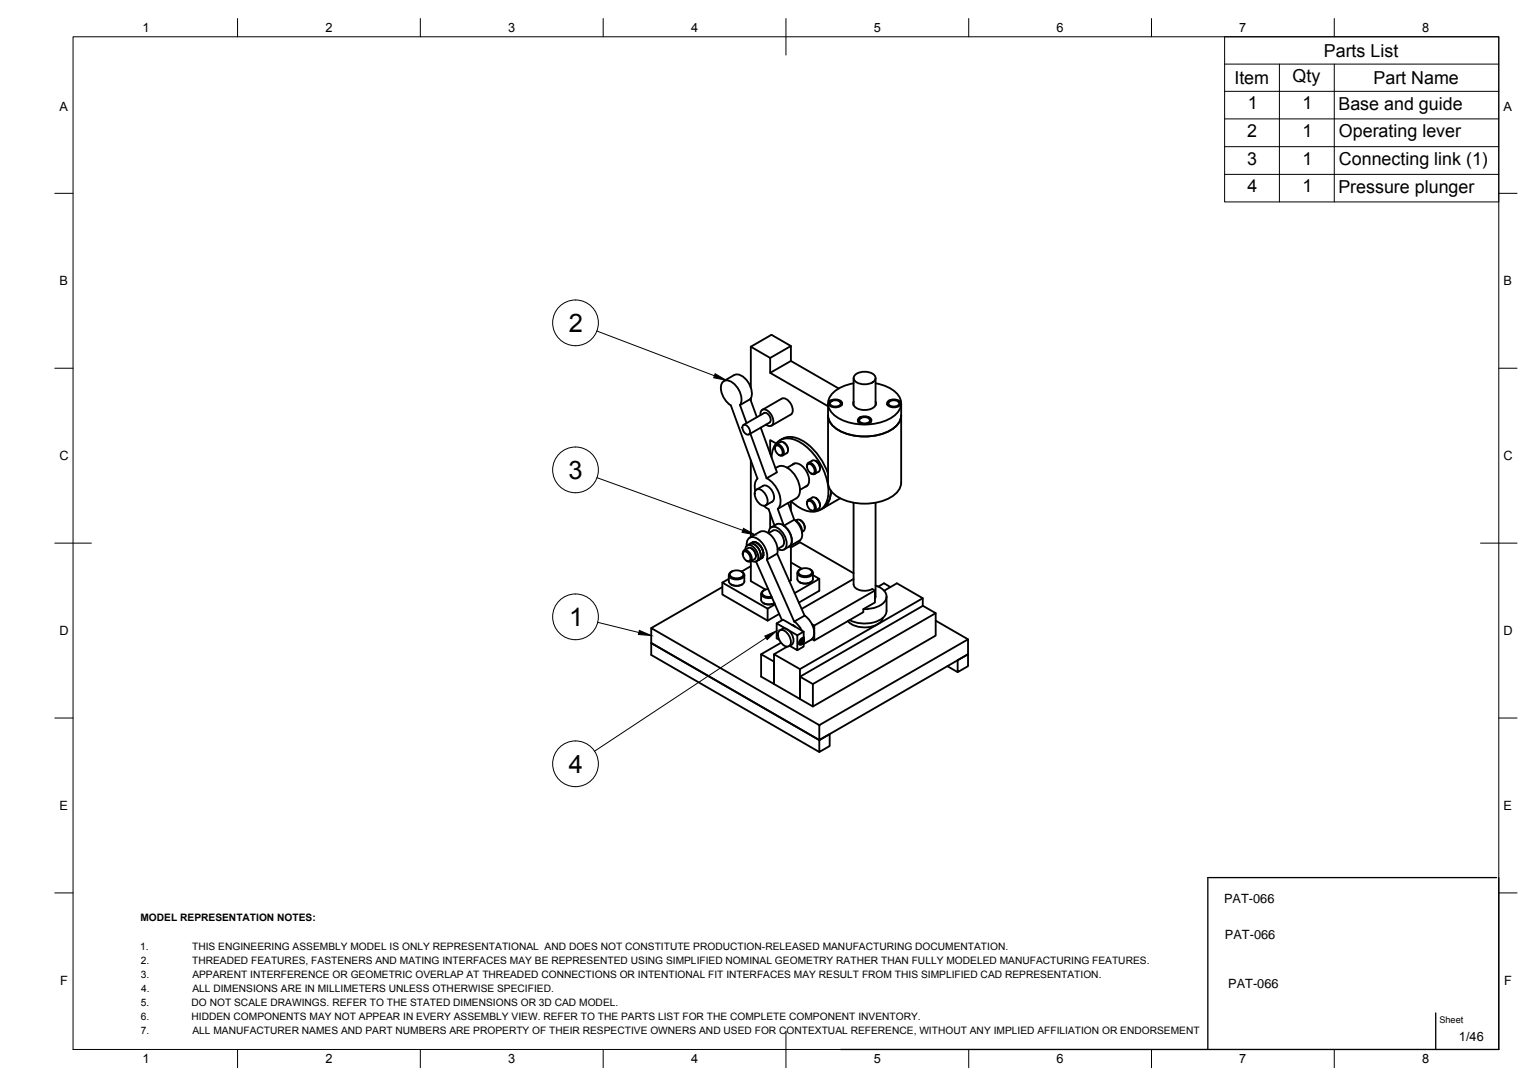
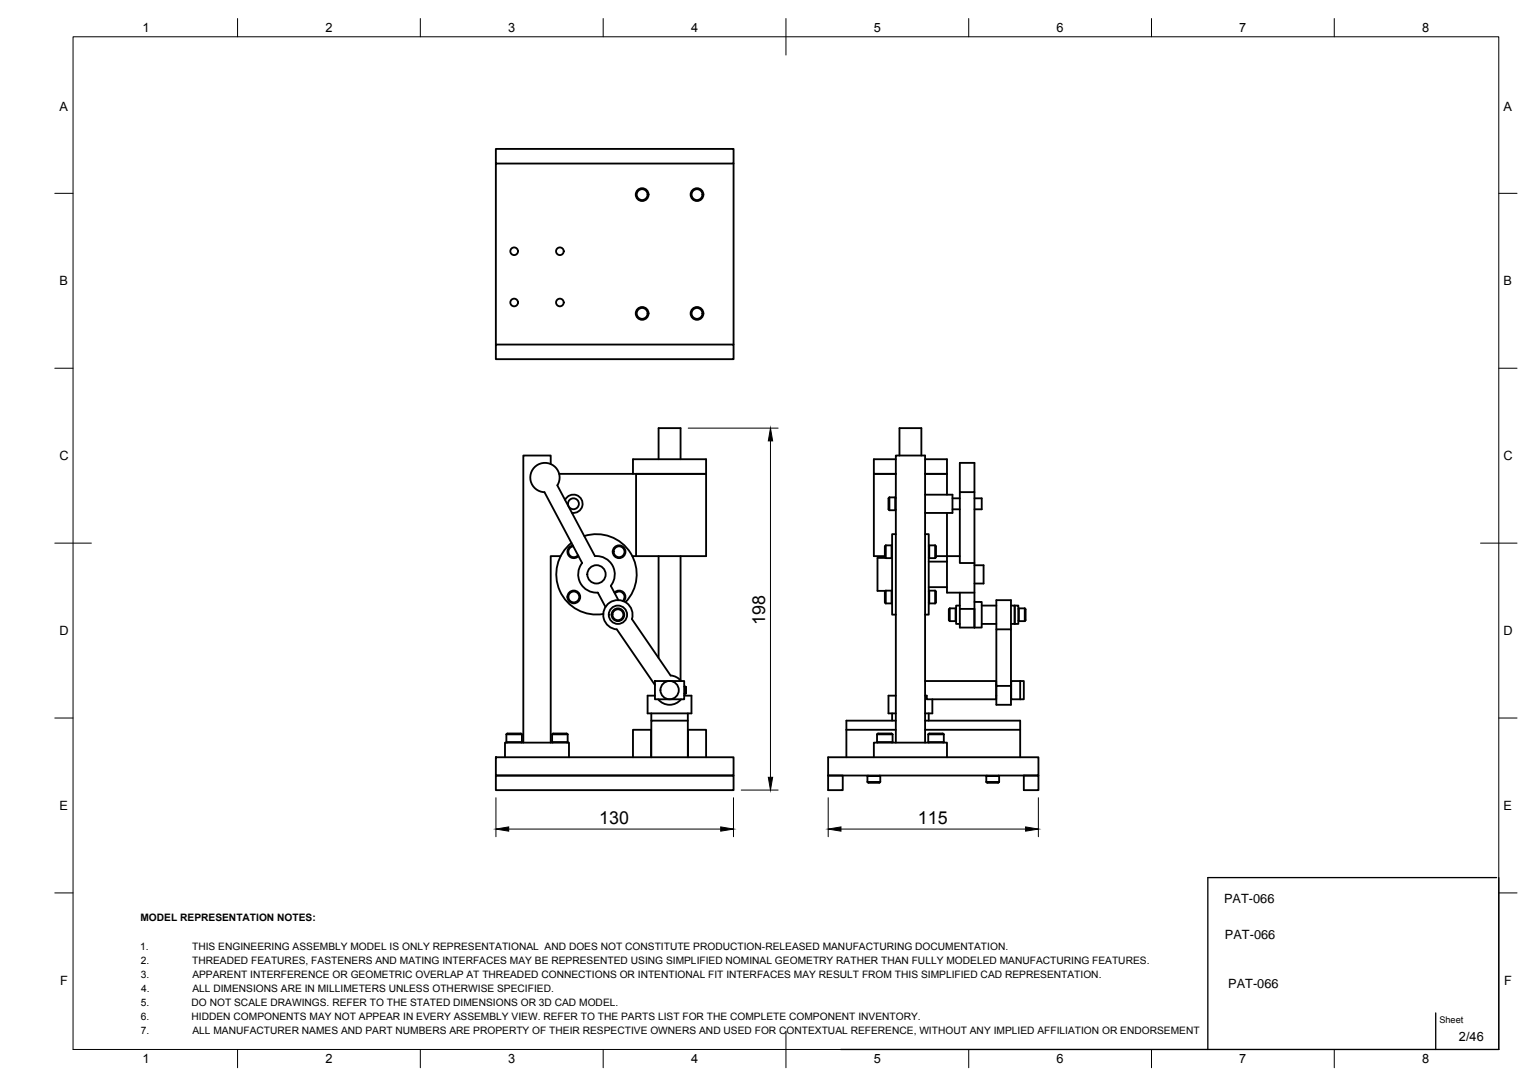
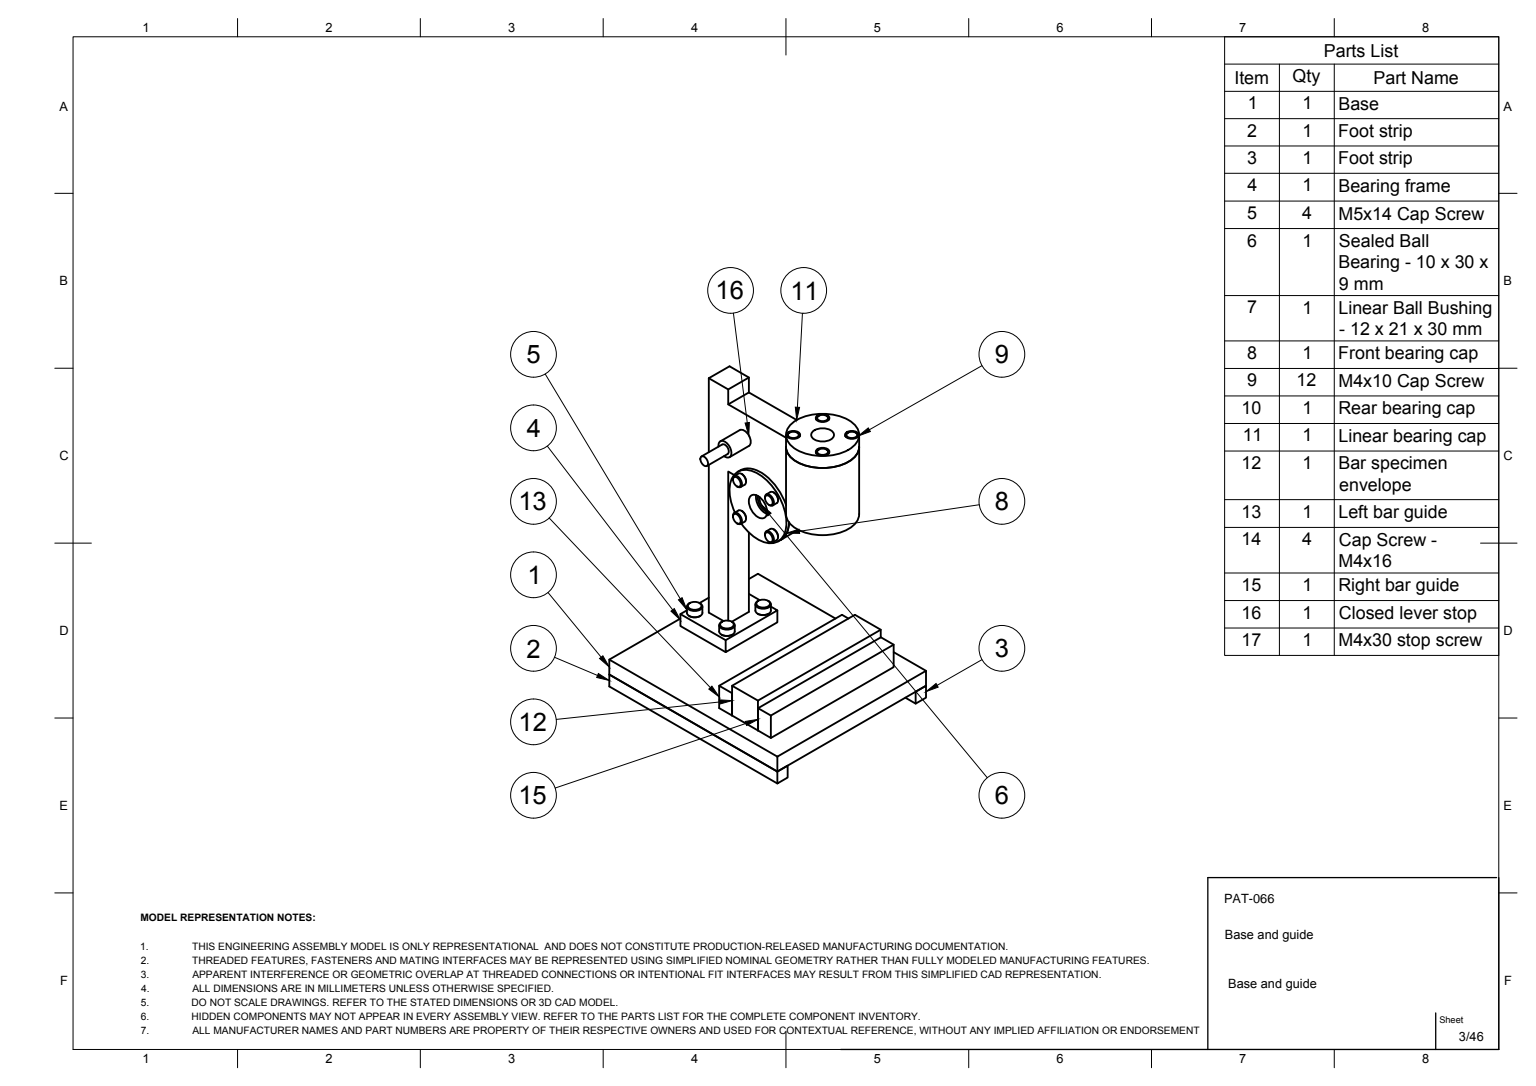
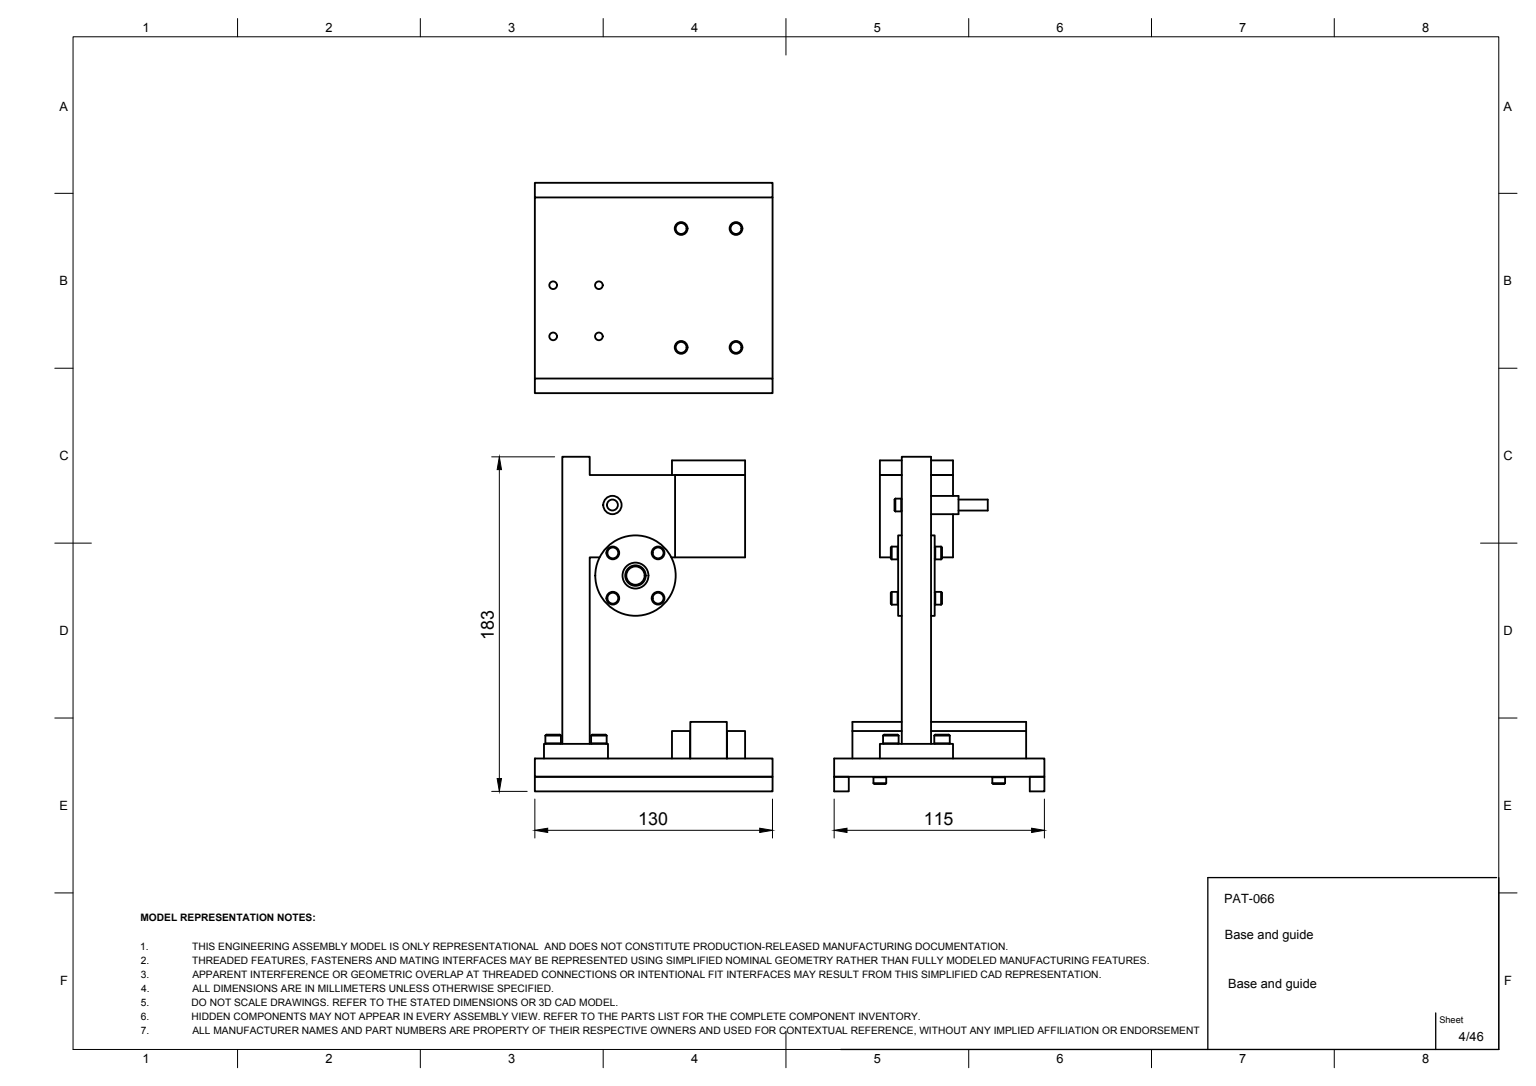
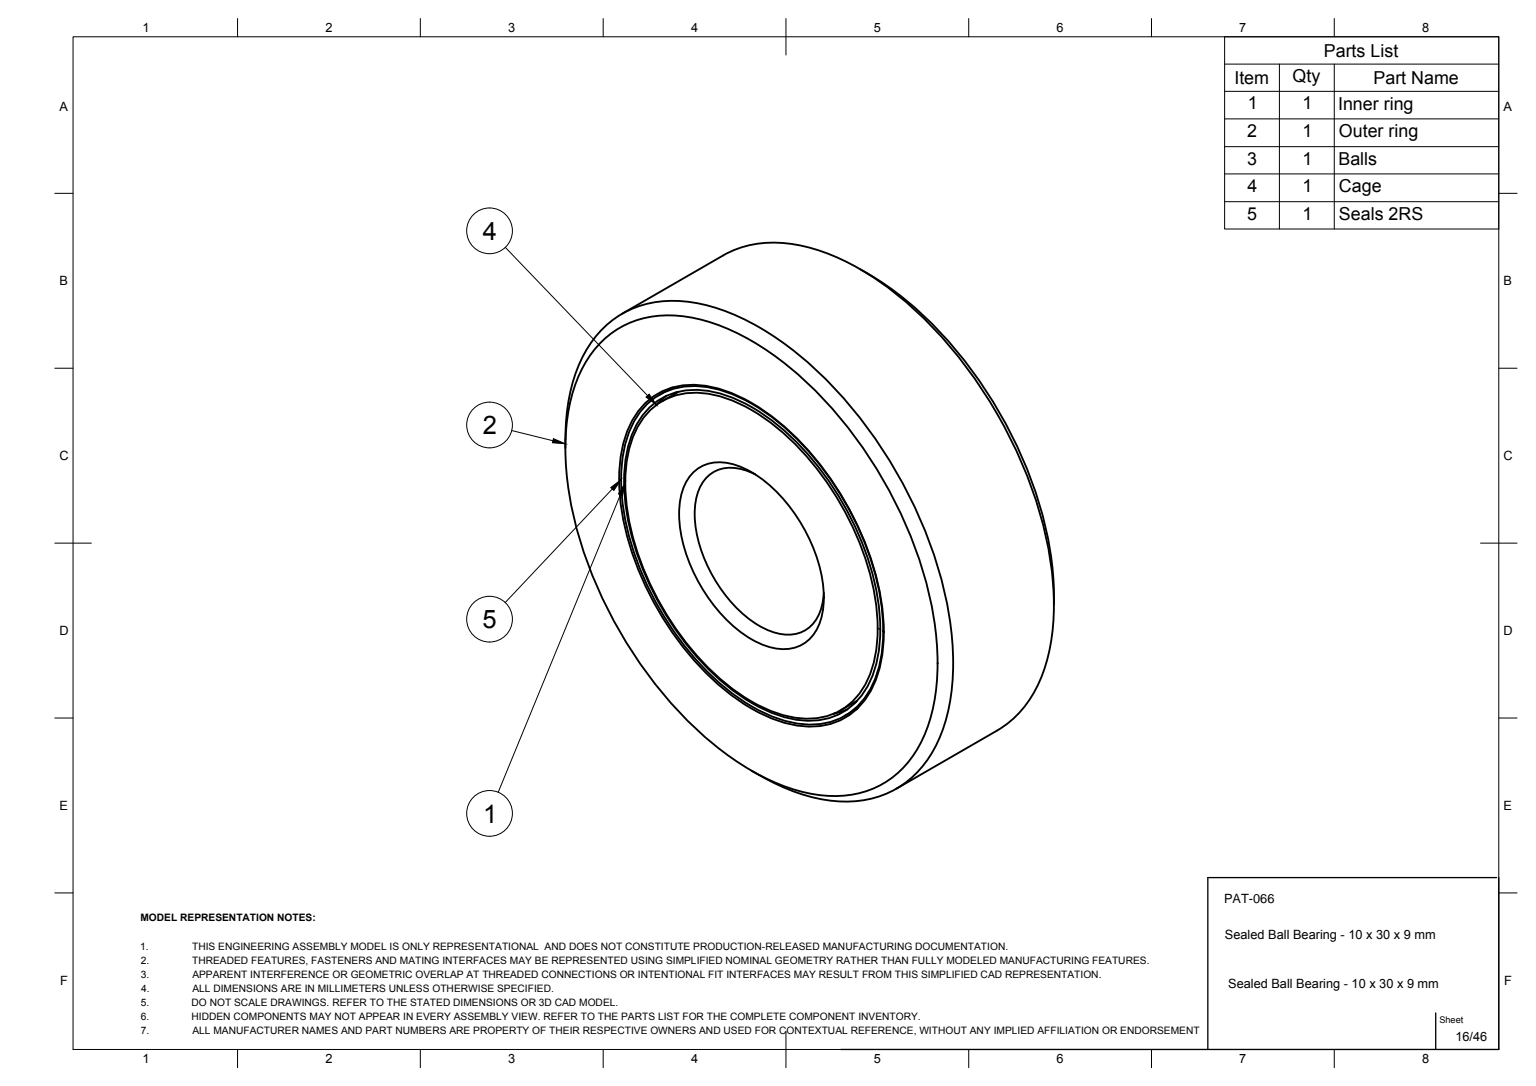
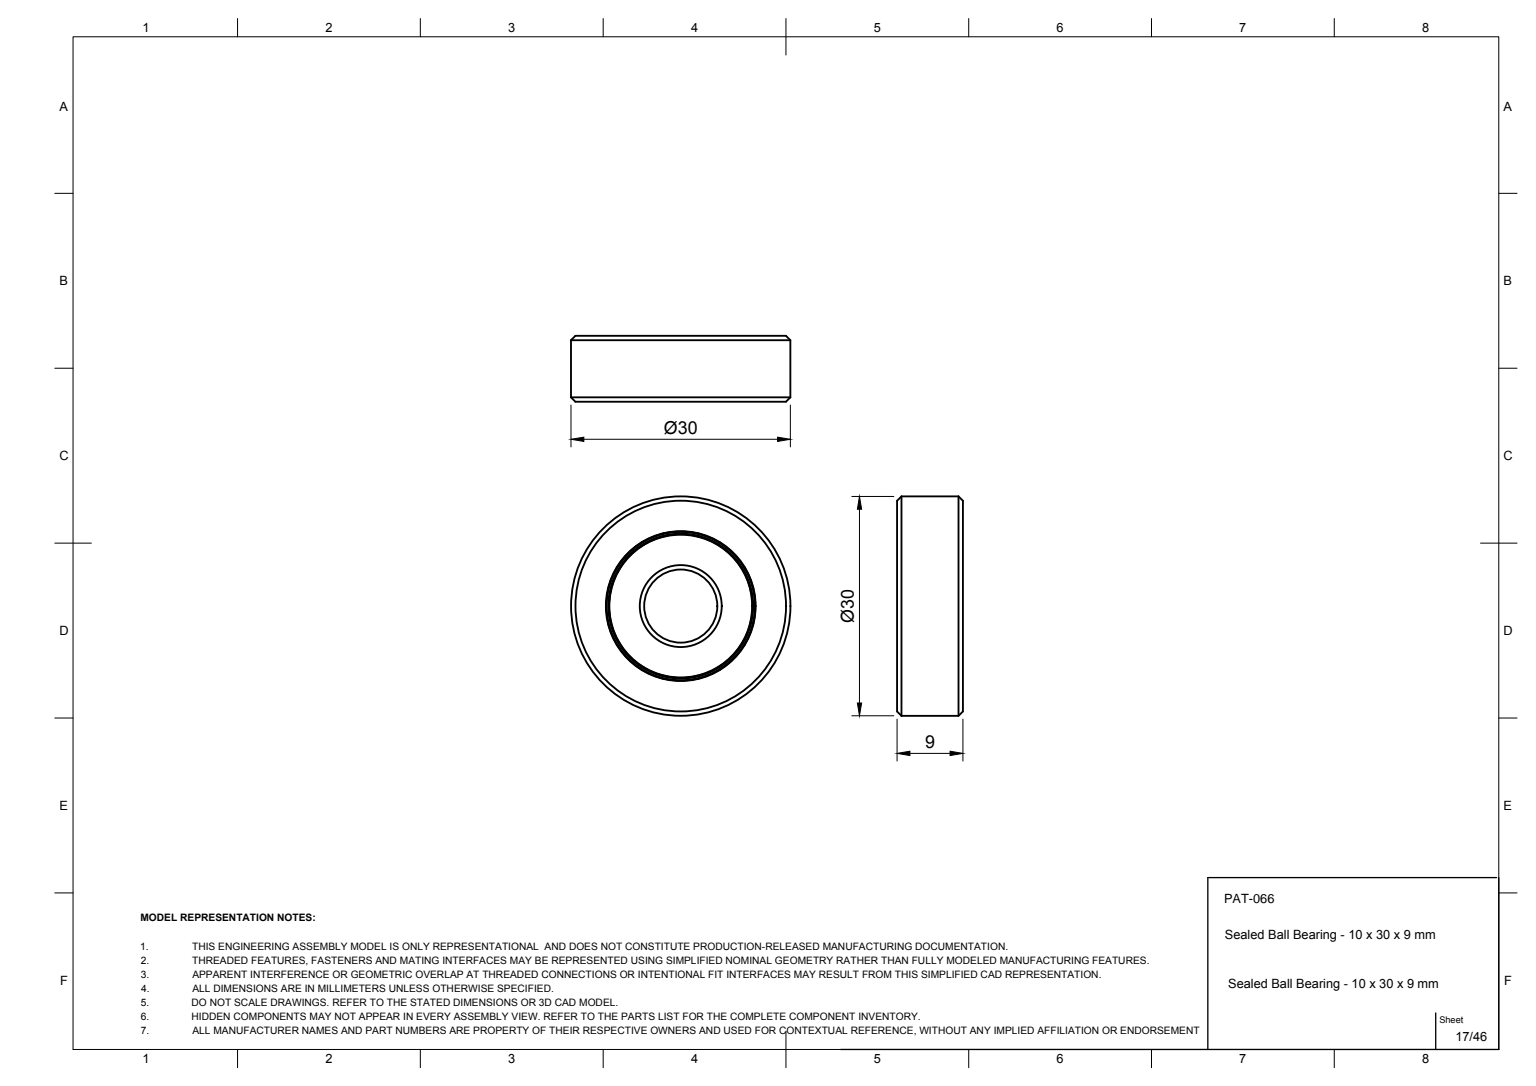
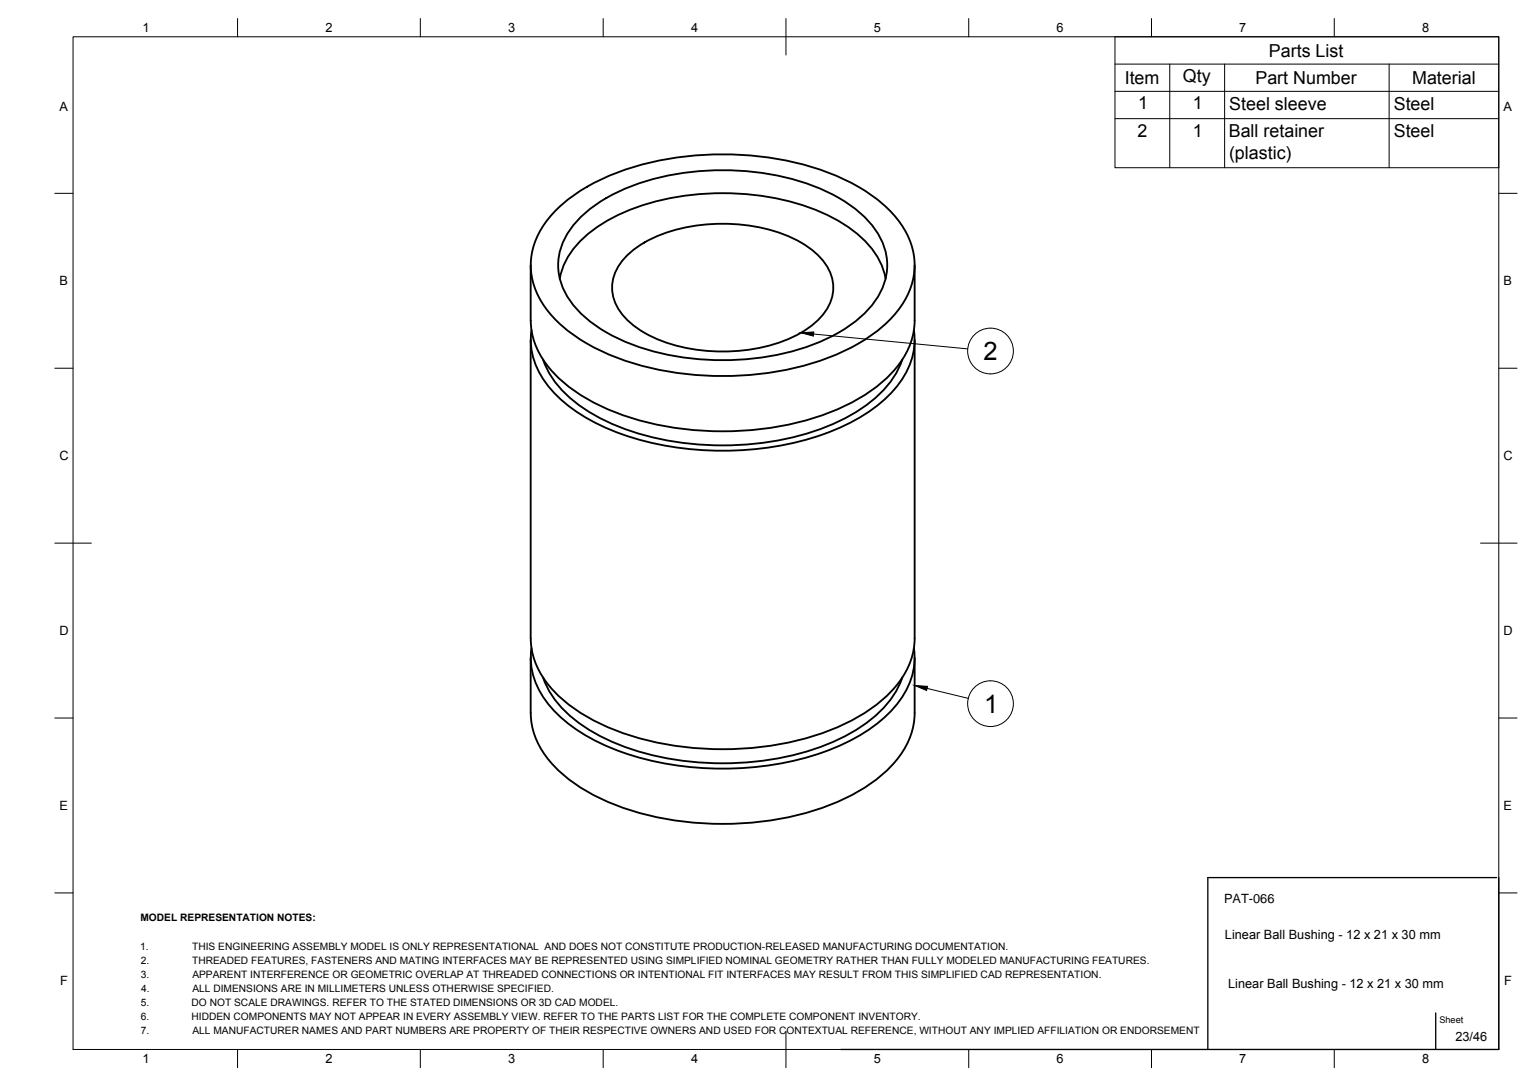
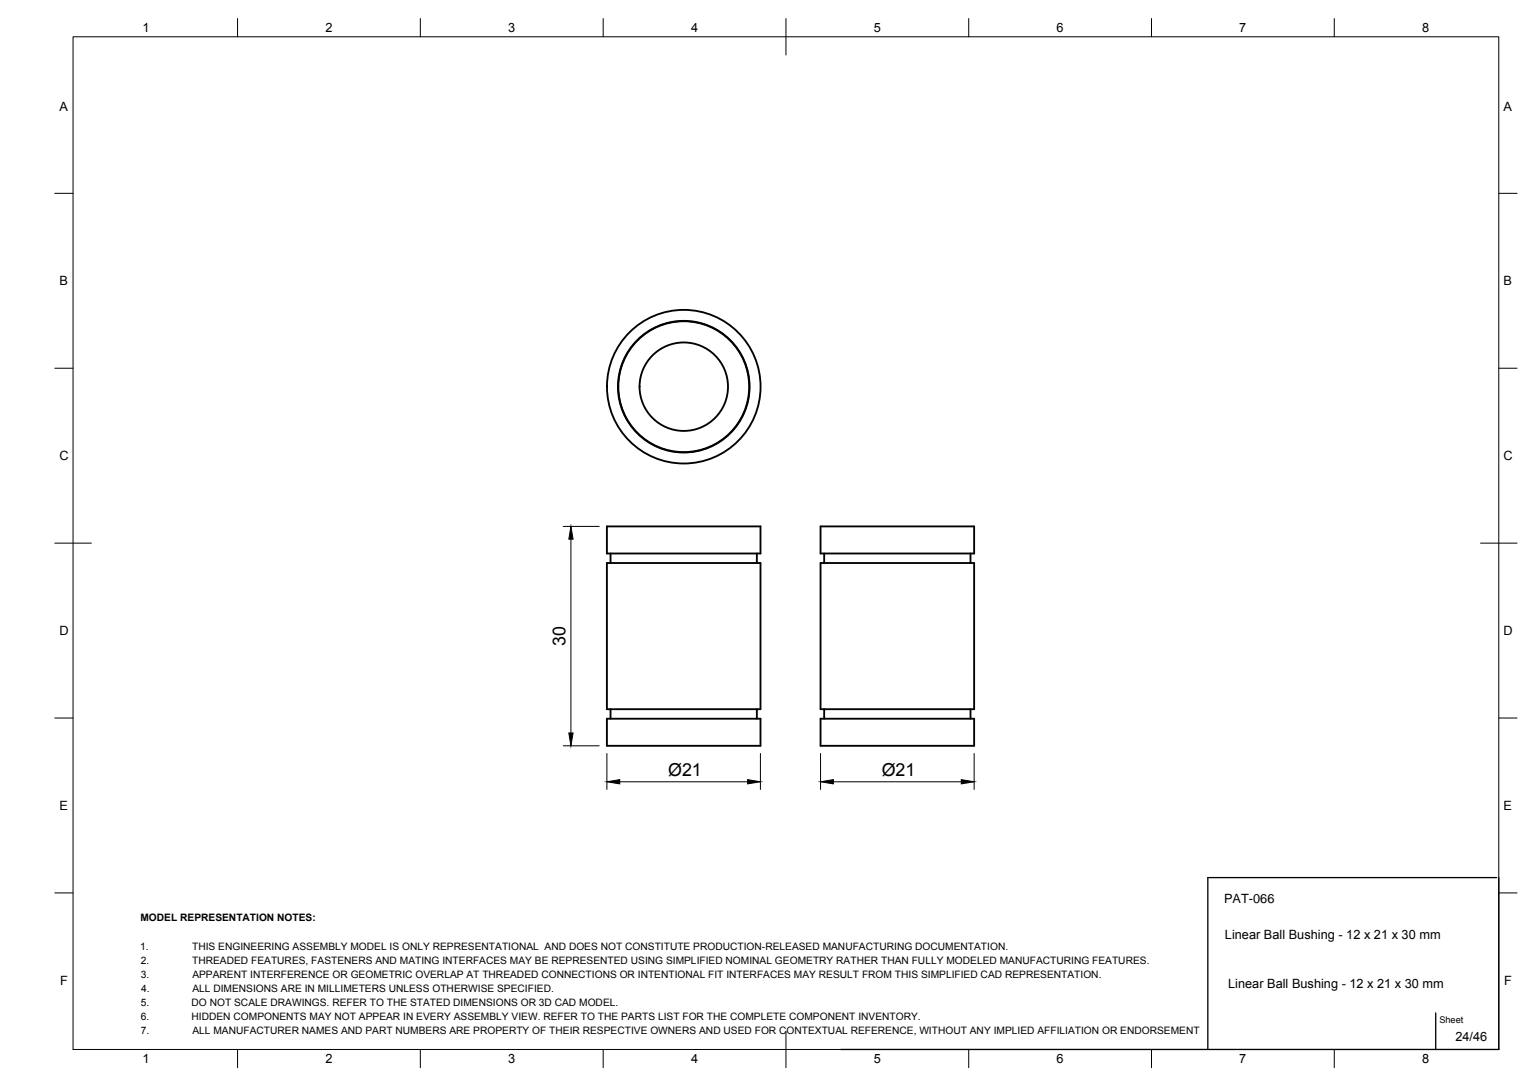
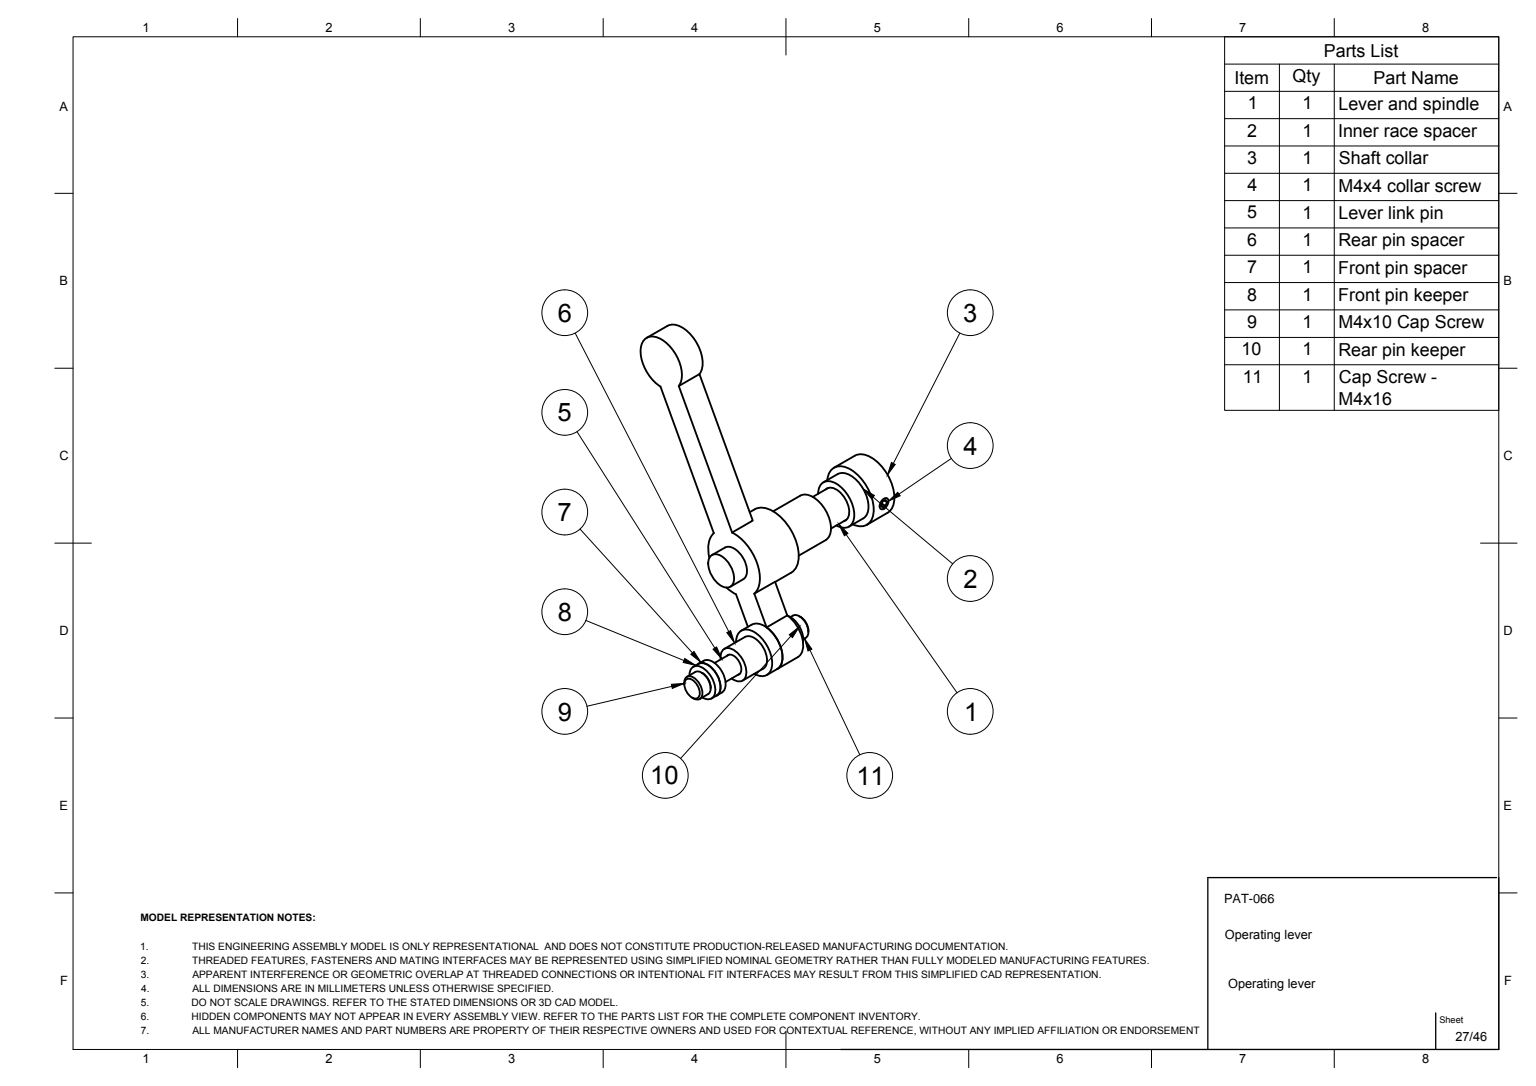
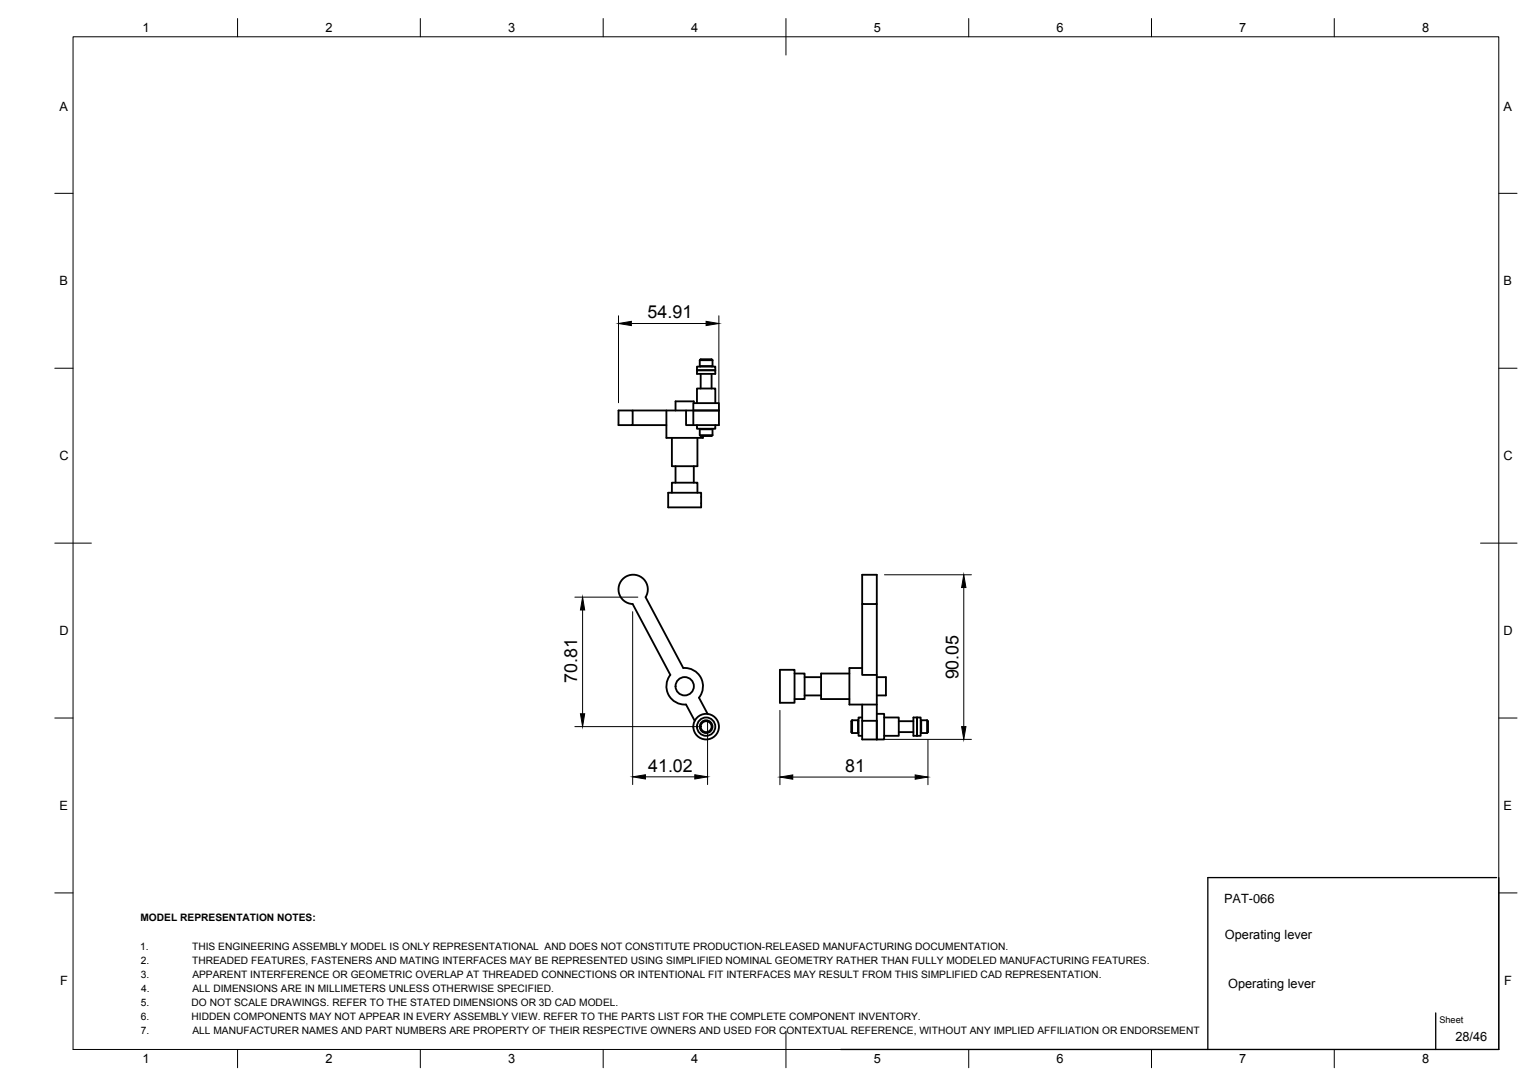
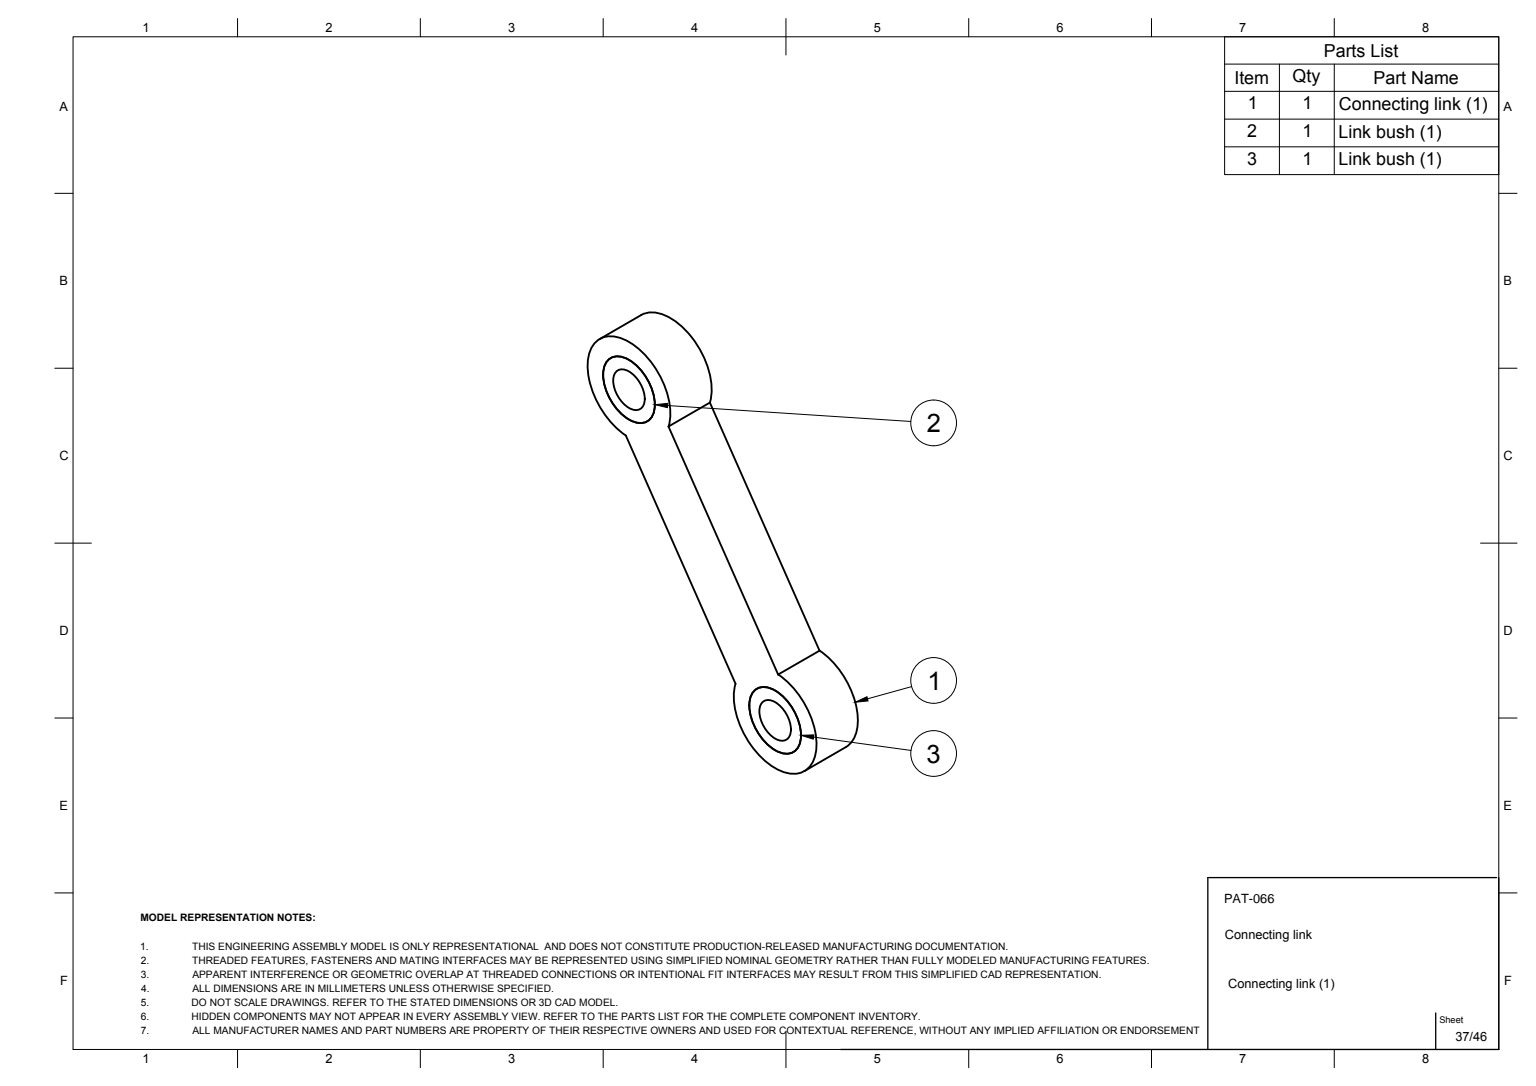
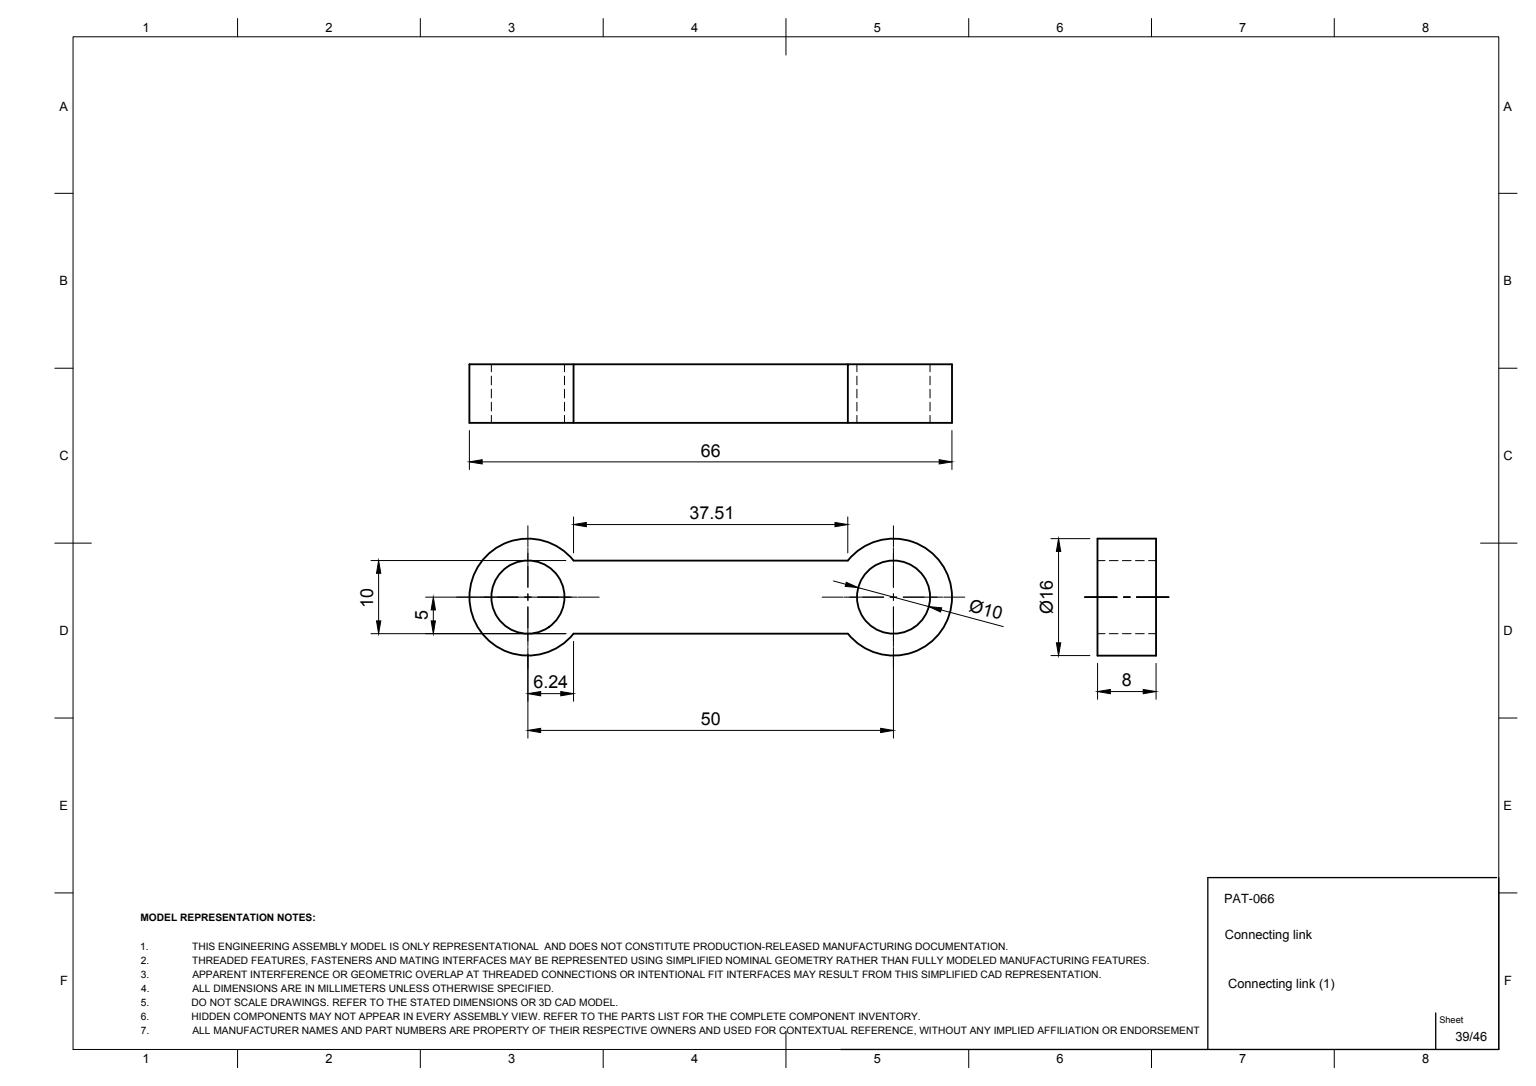
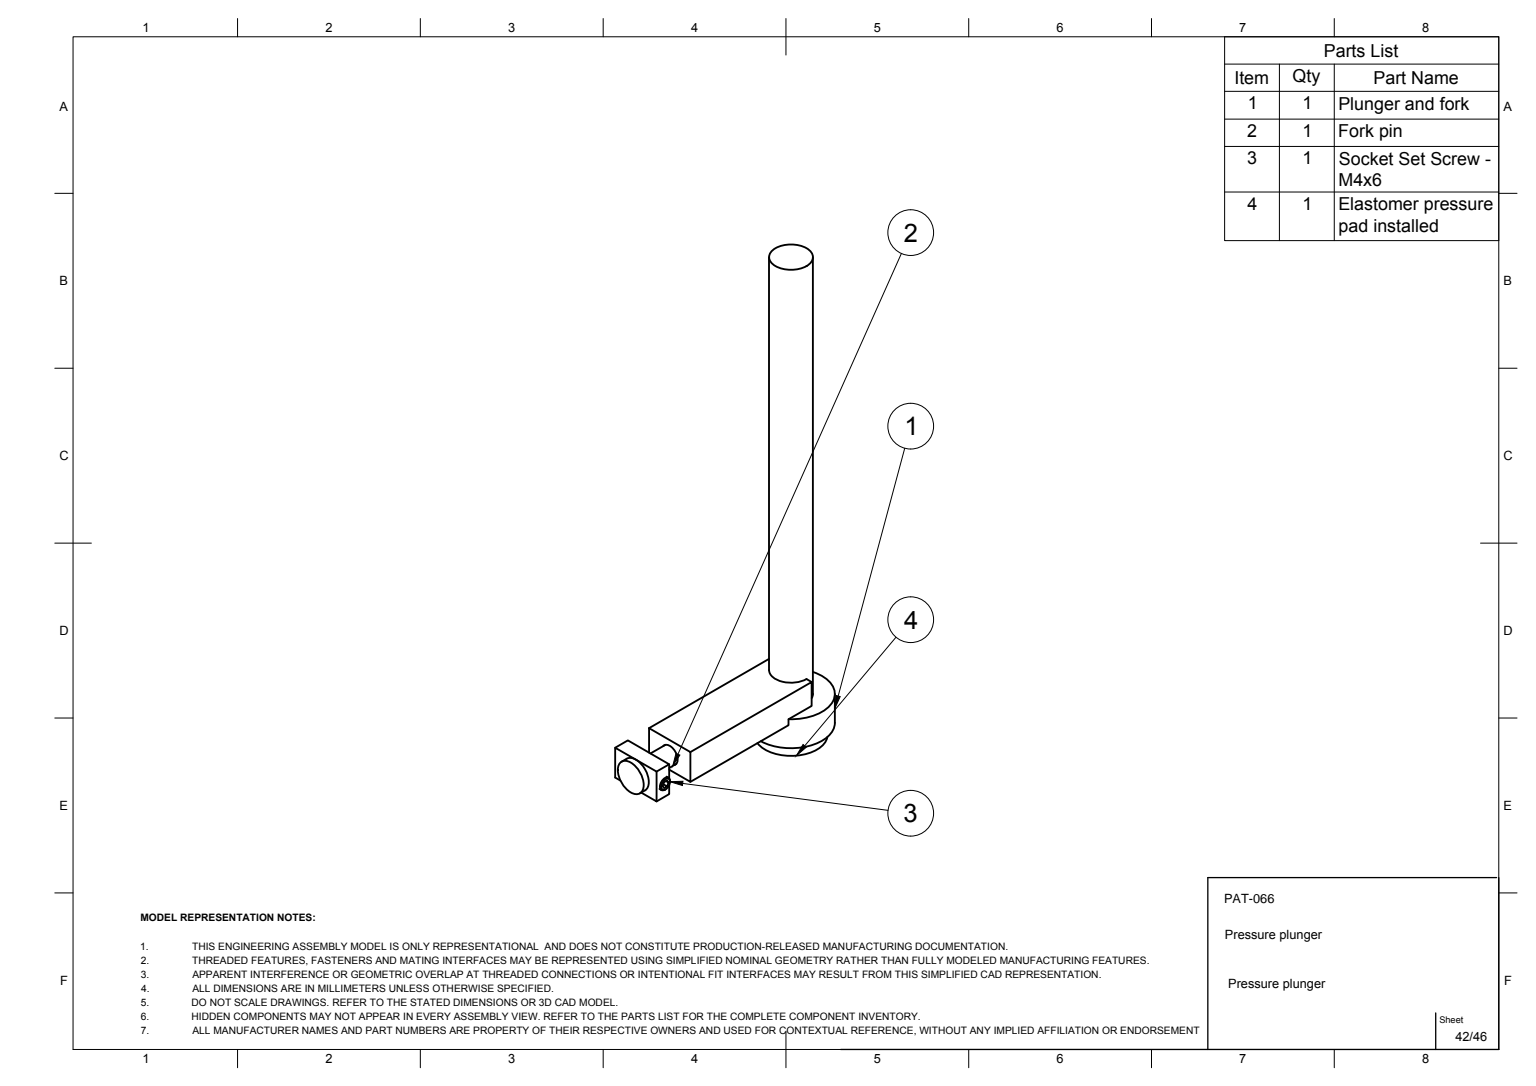
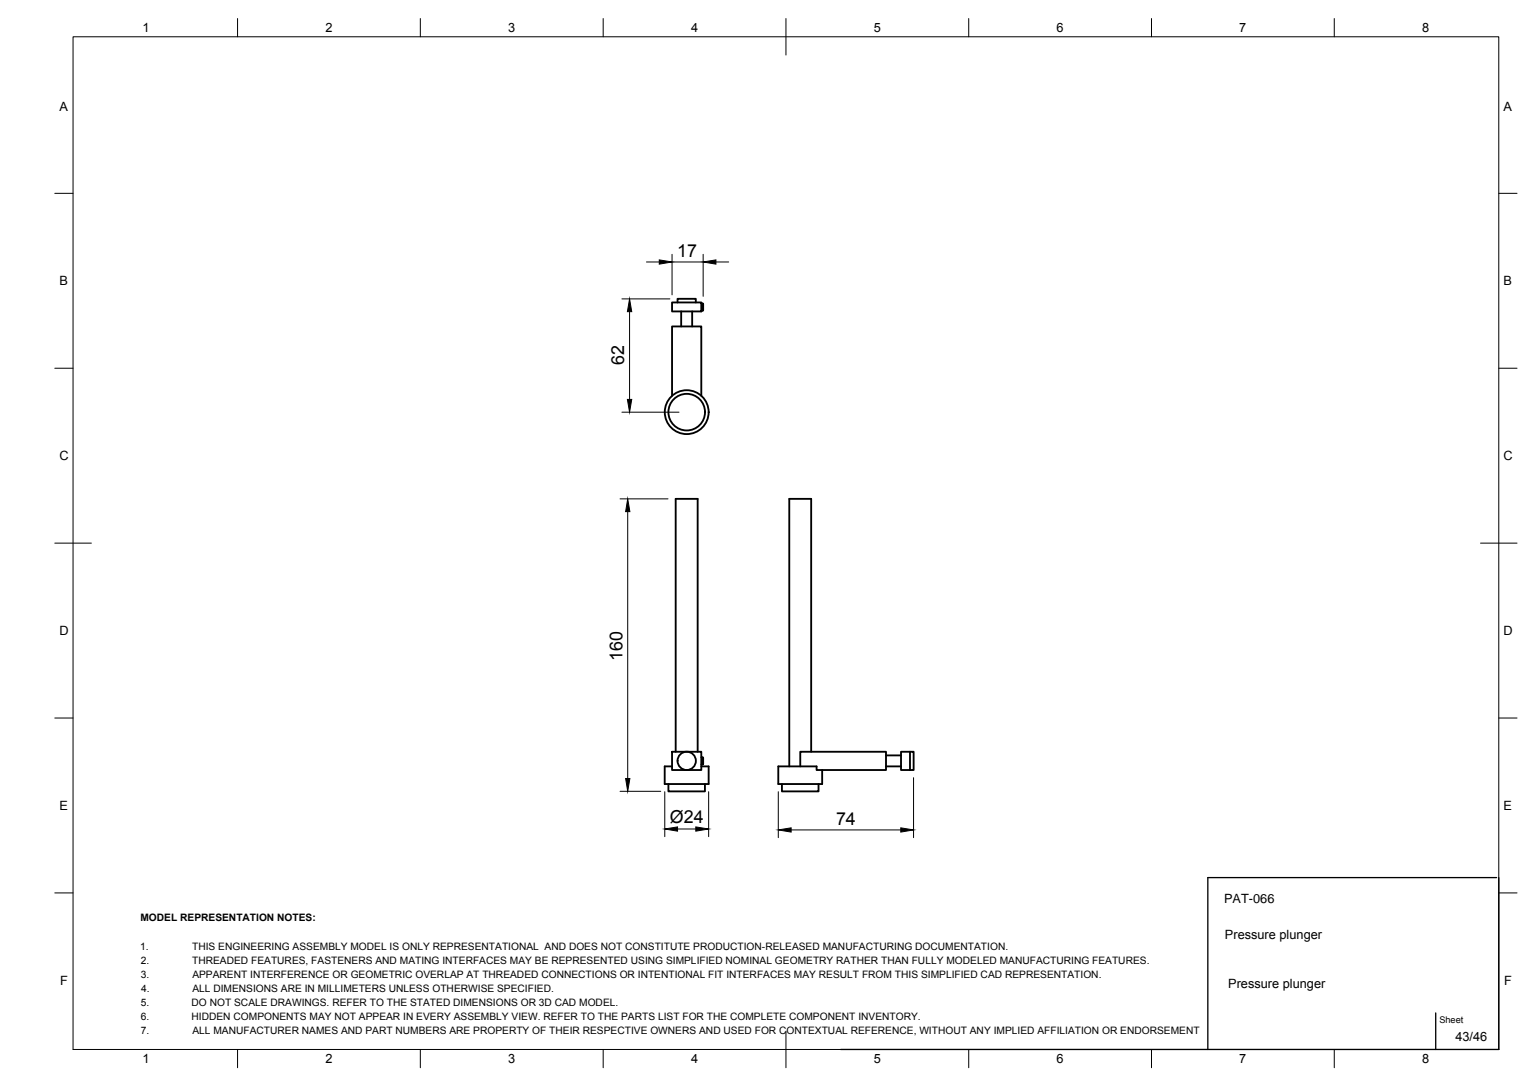
ISO-10303-21;
HEADER;
/* Generated by software containing ST-Developer
 * from STEP Tools, Inc. (www.steptools.com) 
 */

FILE_DESCRIPTION(
/* description */ ('Lever-operated bar clamp (toggle)'),
/* implementation_level */ '2;1');

FILE_NAME(
/* name */ 'PAT-066',
/* time_stamp */ '2026-10-28T03:25:02-07:00',
/* author */ (''),
/* organization */ (''),
/* preprocessor_version */ 'ST-DEVELOPER v20.2',
/* originating_system */ 'Autodesk Translation Framework v15.17.0.0',
/* authorisation */ '');

FILE_SCHEMA (('AUTOMOTIVE_DESIGN { 1 0 10303 214 3 1 1 }'));
ENDSEC;

DATA;
#10=MECHANICAL_DESIGN_GEOMETRIC_PRESENTATION_REPRESENTATION('',(#410,#411,
#412,#413,#414,#415,#416,#417,#418,#419,#420,#421,#422,#423,#424,#425,#426,
#427,#428,#429,#430,#431,#432,#433,#434,#435,#436,#437,#438,#439,#440,#441,
#442,#443,#444,#445,#446,#447,#448,#449,#450,#451,#452,#453,#454,#455,#456),
#12413);
#11=ITEM_DEFINED_TRANSFORMATION($,$,#7328,#7456);
#12=ITEM_DEFINED_TRANSFORMATION($,$,#7348,#7457);
#13=ITEM_DEFINED_TRANSFORMATION($,$,#7368,#7458);
#14=ITEM_DEFINED_TRANSFORMATION($,$,#7385,#7459);
#15=ITEM_DEFINED_TRANSFORMATION($,$,#7439,#7460);
#16=ITEM_DEFINED_TRANSFORMATION($,$,#7462,#7511);
#17=ITEM_DEFINED_TRANSFORMATION($,$,#7494,#7512);
#18=ITEM_DEFINED_TRANSFORMATION($,$,#7041,#7728);
#19=ITEM_DEFINED_TRANSFORMATION($,$,#7072,#7729);
#20=ITEM_DEFINED_TRANSFORMATION($,$,#7079,#7730);
#21=ITEM_DEFINED_TRANSFORMATION($,$,#7086,#7731);
#22=ITEM_DEFINED_TRANSFORMATION($,$,#7161,#7732);
#23=ITEM_DEFINED_TRANSFORMATION($,$,#7186,#7733);
#24=ITEM_DEFINED_TRANSFORMATION($,$,#7211,#7734);
#25=ITEM_DEFINED_TRANSFORMATION($,$,#7252,#7735);
#26=ITEM_DEFINED_TRANSFORMATION($,$,#7259,#7736);
#27=ITEM_DEFINED_TRANSFORMATION($,$,#7274,#7737);
#28=ITEM_DEFINED_TRANSFORMATION($,$,#7289,#7738);
#29=ITEM_DEFINED_TRANSFORMATION($,$,#7303,#7739);
#30=ITEM_DEFINED_TRANSFORMATION($,$,#7303,#7740);
#31=ITEM_DEFINED_TRANSFORMATION($,$,#7303,#7741);
#32=ITEM_DEFINED_TRANSFORMATION($,$,#7303,#7742);
#33=ITEM_DEFINED_TRANSFORMATION($,$,#7327,#7743);
#34=ITEM_DEFINED_TRANSFORMATION($,$,#7461,#7744);
#35=ITEM_DEFINED_TRANSFORMATION($,$,#7678,#7745);
#36=ITEM_DEFINED_TRANSFORMATION($,$,#7678,#7746);
#37=ITEM_DEFINED_TRANSFORMATION($,$,#7678,#7747);
#38=ITEM_DEFINED_TRANSFORMATION($,$,#7678,#7748);
#39=ITEM_DEFINED_TRANSFORMATION($,$,#7678,#7749);
#40=ITEM_DEFINED_TRANSFORMATION($,$,#7678,#7750);
#41=ITEM_DEFINED_TRANSFORMATION($,$,#7678,#7751);
#42=ITEM_DEFINED_TRANSFORMATION($,$,#7678,#7752);
#43=ITEM_DEFINED_TRANSFORMATION($,$,#7678,#7753);
#44=ITEM_DEFINED_TRANSFORMATION($,$,#7678,#7754);
#45=ITEM_DEFINED_TRANSFORMATION($,$,#7678,#7755);
#46=ITEM_DEFINED_TRANSFORMATION($,$,#7678,#7756);
#47=ITEM_DEFINED_TRANSFORMATION($,$,#7702,#7757);
#48=ITEM_DEFINED_TRANSFORMATION($,$,#7702,#7758);
#49=ITEM_DEFINED_TRANSFORMATION($,$,#7702,#7759);
#50=ITEM_DEFINED_TRANSFORMATION($,$,#7702,#7760);
#51=ITEM_DEFINED_TRANSFORMATION($,$,#7513,#7761);
#52=ITEM_DEFINED_TRANSFORMATION($,$,#7544,#7762);
#53=ITEM_DEFINED_TRANSFORMATION($,$,#7581,#7763);
#54=ITEM_DEFINED_TRANSFORMATION($,$,#7590,#7764);
#55=ITEM_DEFINED_TRANSFORMATION($,$,#7605,#7765);
#56=ITEM_DEFINED_TRANSFORMATION($,$,#7627,#7766);
#57=ITEM_DEFINED_TRANSFORMATION($,$,#7636,#7767);
#58=ITEM_DEFINED_TRANSFORMATION($,$,#7645,#7768);
#59=ITEM_DEFINED_TRANSFORMATION($,$,#7654,#7769);
#60=ITEM_DEFINED_TRANSFORMATION($,$,#7663,#7770);
#61=ITEM_DEFINED_TRANSFORMATION($,$,#7678,#7771);
#62=ITEM_DEFINED_TRANSFORMATION($,$,#7702,#7772);
#63=ITEM_DEFINED_TRANSFORMATION($,$,#7774,#7809);
#64=ITEM_DEFINED_TRANSFORMATION($,$,#7791,#7810);
#65=ITEM_DEFINED_TRANSFORMATION($,$,#7800,#7811);
#66=ITEM_DEFINED_TRANSFORMATION($,$,#7813,#7886);
#67=ITEM_DEFINED_TRANSFORMATION($,$,#7853,#7887);
#68=ITEM_DEFINED_TRANSFORMATION($,$,#7863,#7888);
#69=ITEM_DEFINED_TRANSFORMATION($,$,#7869,#7889);
#70=ITEM_DEFINED_TRANSFORMATION($,$,#7040,#7890);
#71=ITEM_DEFINED_TRANSFORMATION($,$,#7543,#7891);
#72=ITEM_DEFINED_TRANSFORMATION($,$,#7773,#7892);
#73=ITEM_DEFINED_TRANSFORMATION($,$,#7812,#7893);
#74=(
REPRESENTATION_RELATIONSHIP($,$,#12586,#12585)
REPRESENTATION_RELATIONSHIP_WITH_TRANSFORMATION(#11)
SHAPE_REPRESENTATION_RELATIONSHIP()
);
#75=(
REPRESENTATION_RELATIONSHIP($,$,#12587,#12585)
REPRESENTATION_RELATIONSHIP_WITH_TRANSFORMATION(#12)
SHAPE_REPRESENTATION_RELATIONSHIP()
);
#76=(
REPRESENTATION_RELATIONSHIP($,$,#12588,#12585)
REPRESENTATION_RELATIONSHIP_WITH_TRANSFORMATION(#13)
SHAPE_REPRESENTATION_RELATIONSHIP()
);
#77=(
REPRESENTATION_RELATIONSHIP($,$,#12589,#12585)
REPRESENTATION_RELATIONSHIP_WITH_TRANSFORMATION(#14)
SHAPE_REPRESENTATION_RELATIONSHIP()
);
#78=(
REPRESENTATION_RELATIONSHIP($,$,#12590,#12585)
REPRESENTATION_RELATIONSHIP_WITH_TRANSFORMATION(#15)
SHAPE_REPRESENTATION_RELATIONSHIP()
);
#79=(
REPRESENTATION_RELATIONSHIP($,$,#12592,#12591)
REPRESENTATION_RELATIONSHIP_WITH_TRANSFORMATION(#16)
SHAPE_REPRESENTATION_RELATIONSHIP()
);
#80=(
REPRESENTATION_RELATIONSHIP($,$,#12593,#12591)
REPRESENTATION_RELATIONSHIP_WITH_TRANSFORMATION(#17)
SHAPE_REPRESENTATION_RELATIONSHIP()
);
#81=(
REPRESENTATION_RELATIONSHIP($,$,#12573,#12572)
REPRESENTATION_RELATIONSHIP_WITH_TRANSFORMATION(#18)
SHAPE_REPRESENTATION_RELATIONSHIP()
);
#82=(
REPRESENTATION_RELATIONSHIP($,$,#12574,#12572)
REPRESENTATION_RELATIONSHIP_WITH_TRANSFORMATION(#19)
SHAPE_REPRESENTATION_RELATIONSHIP()
);
#83=(
REPRESENTATION_RELATIONSHIP($,$,#12575,#12572)
REPRESENTATION_RELATIONSHIP_WITH_TRANSFORMATION(#20)
SHAPE_REPRESENTATION_RELATIONSHIP()
);
#84=(
REPRESENTATION_RELATIONSHIP($,$,#12576,#12572)
REPRESENTATION_RELATIONSHIP_WITH_TRANSFORMATION(#21)
SHAPE_REPRESENTATION_RELATIONSHIP()
);
#85=(
REPRESENTATION_RELATIONSHIP($,$,#12577,#12572)
REPRESENTATION_RELATIONSHIP_WITH_TRANSFORMATION(#22)
SHAPE_REPRESENTATION_RELATIONSHIP()
);
#86=(
REPRESENTATION_RELATIONSHIP($,$,#12578,#12572)
REPRESENTATION_RELATIONSHIP_WITH_TRANSFORMATION(#23)
SHAPE_REPRESENTATION_RELATIONSHIP()
);
#87=(
REPRESENTATION_RELATIONSHIP($,$,#12579,#12572)
REPRESENTATION_RELATIONSHIP_WITH_TRANSFORMATION(#24)
SHAPE_REPRESENTATION_RELATIONSHIP()
);
#88=(
REPRESENTATION_RELATIONSHIP($,$,#12580,#12572)
REPRESENTATION_RELATIONSHIP_WITH_TRANSFORMATION(#25)
SHAPE_REPRESENTATION_RELATIONSHIP()
);
#89=(
REPRESENTATION_RELATIONSHIP($,$,#12581,#12572)
REPRESENTATION_RELATIONSHIP_WITH_TRANSFORMATION(#26)
SHAPE_REPRESENTATION_RELATIONSHIP()
);
#90=(
REPRESENTATION_RELATIONSHIP($,$,#12582,#12572)
REPRESENTATION_RELATIONSHIP_WITH_TRANSFORMATION(#27)
SHAPE_REPRESENTATION_RELATIONSHIP()
);
#91=(
REPRESENTATION_RELATIONSHIP($,$,#12583,#12572)
REPRESENTATION_RELATIONSHIP_WITH_TRANSFORMATION(#28)
SHAPE_REPRESENTATION_RELATIONSHIP()
);
#92=(
REPRESENTATION_RELATIONSHIP($,$,#12584,#12572)
REPRESENTATION_RELATIONSHIP_WITH_TRANSFORMATION(#29)
SHAPE_REPRESENTATION_RELATIONSHIP()
);
#93=(
REPRESENTATION_RELATIONSHIP($,$,#12584,#12572)
REPRESENTATION_RELATIONSHIP_WITH_TRANSFORMATION(#30)
SHAPE_REPRESENTATION_RELATIONSHIP()
);
#94=(
REPRESENTATION_RELATIONSHIP($,$,#12584,#12572)
REPRESENTATION_RELATIONSHIP_WITH_TRANSFORMATION(#31)
SHAPE_REPRESENTATION_RELATIONSHIP()
);
#95=(
REPRESENTATION_RELATIONSHIP($,$,#12584,#12572)
REPRESENTATION_RELATIONSHIP_WITH_TRANSFORMATION(#32)
SHAPE_REPRESENTATION_RELATIONSHIP()
);
#96=(
REPRESENTATION_RELATIONSHIP($,$,#12585,#12572)
REPRESENTATION_RELATIONSHIP_WITH_TRANSFORMATION(#33)
SHAPE_REPRESENTATION_RELATIONSHIP()
);
#97=(
REPRESENTATION_RELATIONSHIP($,$,#12591,#12572)
REPRESENTATION_RELATIONSHIP_WITH_TRANSFORMATION(#34)
SHAPE_REPRESENTATION_RELATIONSHIP()
);
#98=(
REPRESENTATION_RELATIONSHIP($,$,#12605,#12572)
REPRESENTATION_RELATIONSHIP_WITH_TRANSFORMATION(#35)
SHAPE_REPRESENTATION_RELATIONSHIP()
);
#99=(
REPRESENTATION_RELATIONSHIP($,$,#12605,#12572)
REPRESENTATION_RELATIONSHIP_WITH_TRANSFORMATION(#36)
SHAPE_REPRESENTATION_RELATIONSHIP()
);
#100=(
REPRESENTATION_RELATIONSHIP($,$,#12605,#12572)
REPRESENTATION_RELATIONSHIP_WITH_TRANSFORMATION(#37)
SHAPE_REPRESENTATION_RELATIONSHIP()
);
#101=(
REPRESENTATION_RELATIONSHIP($,$,#12605,#12572)
REPRESENTATION_RELATIONSHIP_WITH_TRANSFORMATION(#38)
SHAPE_REPRESENTATION_RELATIONSHIP()
);
#102=(
REPRESENTATION_RELATIONSHIP($,$,#12605,#12572)
REPRESENTATION_RELATIONSHIP_WITH_TRANSFORMATION(#39)
SHAPE_REPRESENTATION_RELATIONSHIP()
);
#103=(
REPRESENTATION_RELATIONSHIP($,$,#12605,#12572)
REPRESENTATION_RELATIONSHIP_WITH_TRANSFORMATION(#40)
SHAPE_REPRESENTATION_RELATIONSHIP()
);
#104=(
REPRESENTATION_RELATIONSHIP($,$,#12605,#12572)
REPRESENTATION_RELATIONSHIP_WITH_TRANSFORMATION(#41)
SHAPE_REPRESENTATION_RELATIONSHIP()
);
#105=(
REPRESENTATION_RELATIONSHIP($,$,#12605,#12572)
REPRESENTATION_RELATIONSHIP_WITH_TRANSFORMATION(#42)
SHAPE_REPRESENTATION_RELATIONSHIP()
);
#106=(
REPRESENTATION_RELATIONSHIP($,$,#12605,#12572)
REPRESENTATION_RELATIONSHIP_WITH_TRANSFORMATION(#43)
SHAPE_REPRESENTATION_RELATIONSHIP()
);
#107=(
REPRESENTATION_RELATIONSHIP($,$,#12605,#12572)
REPRESENTATION_RELATIONSHIP_WITH_TRANSFORMATION(#44)
SHAPE_REPRESENTATION_RELATIONSHIP()
);
#108=(
REPRESENTATION_RELATIONSHIP($,$,#12605,#12572)
REPRESENTATION_RELATIONSHIP_WITH_TRANSFORMATION(#45)
SHAPE_REPRESENTATION_RELATIONSHIP()
);
#109=(
REPRESENTATION_RELATIONSHIP($,$,#12605,#12572)
REPRESENTATION_RELATIONSHIP_WITH_TRANSFORMATION(#46)
SHAPE_REPRESENTATION_RELATIONSHIP()
);
#110=(
REPRESENTATION_RELATIONSHIP($,$,#12606,#12572)
REPRESENTATION_RELATIONSHIP_WITH_TRANSFORMATION(#47)
SHAPE_REPRESENTATION_RELATIONSHIP()
);
#111=(
REPRESENTATION_RELATIONSHIP($,$,#12606,#12572)
REPRESENTATION_RELATIONSHIP_WITH_TRANSFORMATION(#48)
SHAPE_REPRESENTATION_RELATIONSHIP()
);
#112=(
REPRESENTATION_RELATIONSHIP($,$,#12606,#12572)
REPRESENTATION_RELATIONSHIP_WITH_TRANSFORMATION(#49)
SHAPE_REPRESENTATION_RELATIONSHIP()
);
#113=(
REPRESENTATION_RELATIONSHIP($,$,#12606,#12572)
REPRESENTATION_RELATIONSHIP_WITH_TRANSFORMATION(#50)
SHAPE_REPRESENTATION_RELATIONSHIP()
);
#114=(
REPRESENTATION_RELATIONSHIP($,$,#12594,#12572)
REPRESENTATION_RELATIONSHIP_WITH_TRANSFORMATION(#51)
SHAPE_REPRESENTATION_RELATIONSHIP()
);
#115=(
REPRESENTATION_RELATIONSHIP($,$,#12596,#12595)
REPRESENTATION_RELATIONSHIP_WITH_TRANSFORMATION(#52)
SHAPE_REPRESENTATION_RELATIONSHIP()
);
#116=(
REPRESENTATION_RELATIONSHIP($,$,#12597,#12595)
REPRESENTATION_RELATIONSHIP_WITH_TRANSFORMATION(#53)
SHAPE_REPRESENTATION_RELATIONSHIP()
);
#117=(
REPRESENTATION_RELATIONSHIP($,$,#12598,#12595)
REPRESENTATION_RELATIONSHIP_WITH_TRANSFORMATION(#54)
SHAPE_REPRESENTATION_RELATIONSHIP()
);
#118=(
REPRESENTATION_RELATIONSHIP($,$,#12599,#12595)
REPRESENTATION_RELATIONSHIP_WITH_TRANSFORMATION(#55)
SHAPE_REPRESENTATION_RELATIONSHIP()
);
#119=(
REPRESENTATION_RELATIONSHIP($,$,#12600,#12595)
REPRESENTATION_RELATIONSHIP_WITH_TRANSFORMATION(#56)
SHAPE_REPRESENTATION_RELATIONSHIP()
);
#120=(
REPRESENTATION_RELATIONSHIP($,$,#12601,#12595)
REPRESENTATION_RELATIONSHIP_WITH_TRANSFORMATION(#57)
SHAPE_REPRESENTATION_RELATIONSHIP()
);
#121=(
REPRESENTATION_RELATIONSHIP($,$,#12602,#12595)
REPRESENTATION_RELATIONSHIP_WITH_TRANSFORMATION(#58)
SHAPE_REPRESENTATION_RELATIONSHIP()
);
#122=(
REPRESENTATION_RELATIONSHIP($,$,#12603,#12595)
REPRESENTATION_RELATIONSHIP_WITH_TRANSFORMATION(#59)
SHAPE_REPRESENTATION_RELATIONSHIP()
);
#123=(
REPRESENTATION_RELATIONSHIP($,$,#12604,#12595)
REPRESENTATION_RELATIONSHIP_WITH_TRANSFORMATION(#60)
SHAPE_REPRESENTATION_RELATIONSHIP()
);
#124=(
REPRESENTATION_RELATIONSHIP($,$,#12605,#12595)
REPRESENTATION_RELATIONSHIP_WITH_TRANSFORMATION(#61)
SHAPE_REPRESENTATION_RELATIONSHIP()
);
#125=(
REPRESENTATION_RELATIONSHIP($,$,#12606,#12595)
REPRESENTATION_RELATIONSHIP_WITH_TRANSFORMATION(#62)
SHAPE_REPRESENTATION_RELATIONSHIP()
);
#126=(
REPRESENTATION_RELATIONSHIP($,$,#12608,#12607)
REPRESENTATION_RELATIONSHIP_WITH_TRANSFORMATION(#63)
SHAPE_REPRESENTATION_RELATIONSHIP()
);
#127=(
REPRESENTATION_RELATIONSHIP($,$,#12609,#12607)
REPRESENTATION_RELATIONSHIP_WITH_TRANSFORMATION(#64)
SHAPE_REPRESENTATION_RELATIONSHIP()
);
#128=(
REPRESENTATION_RELATIONSHIP($,$,#12610,#12607)
REPRESENTATION_RELATIONSHIP_WITH_TRANSFORMATION(#65)
SHAPE_REPRESENTATION_RELATIONSHIP()
);
#129=(
REPRESENTATION_RELATIONSHIP($,$,#12612,#12611)
REPRESENTATION_RELATIONSHIP_WITH_TRANSFORMATION(#66)
SHAPE_REPRESENTATION_RELATIONSHIP()
);
#130=(
REPRESENTATION_RELATIONSHIP($,$,#12613,#12611)
REPRESENTATION_RELATIONSHIP_WITH_TRANSFORMATION(#67)
SHAPE_REPRESENTATION_RELATIONSHIP()
);
#131=(
REPRESENTATION_RELATIONSHIP($,$,#12614,#12611)
REPRESENTATION_RELATIONSHIP_WITH_TRANSFORMATION(#68)
SHAPE_REPRESENTATION_RELATIONSHIP()
);
#132=(
REPRESENTATION_RELATIONSHIP($,$,#12615,#12611)
REPRESENTATION_RELATIONSHIP_WITH_TRANSFORMATION(#69)
SHAPE_REPRESENTATION_RELATIONSHIP()
);
#133=(
REPRESENTATION_RELATIONSHIP($,$,#12572,#12571)
REPRESENTATION_RELATIONSHIP_WITH_TRANSFORMATION(#70)
SHAPE_REPRESENTATION_RELATIONSHIP()
);
#134=(
REPRESENTATION_RELATIONSHIP($,$,#12595,#12571)
REPRESENTATION_RELATIONSHIP_WITH_TRANSFORMATION(#71)
SHAPE_REPRESENTATION_RELATIONSHIP()
);
#135=(
REPRESENTATION_RELATIONSHIP($,$,#12607,#12571)
REPRESENTATION_RELATIONSHIP_WITH_TRANSFORMATION(#72)
SHAPE_REPRESENTATION_RELATIONSHIP()
);
#136=(
REPRESENTATION_RELATIONSHIP($,$,#12611,#12571)
REPRESENTATION_RELATIONSHIP_WITH_TRANSFORMATION(#73)
SHAPE_REPRESENTATION_RELATIONSHIP()
);
#137=CONTEXT_DEPENDENT_SHAPE_REPRESENTATION(#74,#12483);
#138=CONTEXT_DEPENDENT_SHAPE_REPRESENTATION(#75,#12484);
#139=CONTEXT_DEPENDENT_SHAPE_REPRESENTATION(#76,#12485);
#140=CONTEXT_DEPENDENT_SHAPE_REPRESENTATION(#77,#12486);
#141=CONTEXT_DEPENDENT_SHAPE_REPRESENTATION(#78,#12487);
#142=CONTEXT_DEPENDENT_SHAPE_REPRESENTATION(#79,#12491);
#143=CONTEXT_DEPENDENT_SHAPE_REPRESENTATION(#80,#12492);
#144=CONTEXT_DEPENDENT_SHAPE_REPRESENTATION(#81,#12506);
#145=CONTEXT_DEPENDENT_SHAPE_REPRESENTATION(#82,#12507);
#146=CONTEXT_DEPENDENT_SHAPE_REPRESENTATION(#83,#12508);
#147=CONTEXT_DEPENDENT_SHAPE_REPRESENTATION(#84,#12509);
#148=CONTEXT_DEPENDENT_SHAPE_REPRESENTATION(#85,#12510);
#149=CONTEXT_DEPENDENT_SHAPE_REPRESENTATION(#86,#12511);
#150=CONTEXT_DEPENDENT_SHAPE_REPRESENTATION(#87,#12512);
#151=CONTEXT_DEPENDENT_SHAPE_REPRESENTATION(#88,#12513);
#152=CONTEXT_DEPENDENT_SHAPE_REPRESENTATION(#89,#12514);
#153=CONTEXT_DEPENDENT_SHAPE_REPRESENTATION(#90,#12515);
#154=CONTEXT_DEPENDENT_SHAPE_REPRESENTATION(#91,#12516);
#155=CONTEXT_DEPENDENT_SHAPE_REPRESENTATION(#92,#12517);
#156=CONTEXT_DEPENDENT_SHAPE_REPRESENTATION(#93,#12518);
#157=CONTEXT_DEPENDENT_SHAPE_REPRESENTATION(#94,#12519);
#158=CONTEXT_DEPENDENT_SHAPE_REPRESENTATION(#95,#12520);
#159=CONTEXT_DEPENDENT_SHAPE_REPRESENTATION(#96,#12521);
#160=CONTEXT_DEPENDENT_SHAPE_REPRESENTATION(#97,#12522);
#161=CONTEXT_DEPENDENT_SHAPE_REPRESENTATION(#98,#12523);
#162=CONTEXT_DEPENDENT_SHAPE_REPRESENTATION(#99,#12524);
#163=CONTEXT_DEPENDENT_SHAPE_REPRESENTATION(#100,#12525);
#164=CONTEXT_DEPENDENT_SHAPE_REPRESENTATION(#101,#12526);
#165=CONTEXT_DEPENDENT_SHAPE_REPRESENTATION(#102,#12527);
#166=CONTEXT_DEPENDENT_SHAPE_REPRESENTATION(#103,#12528);
#167=CONTEXT_DEPENDENT_SHAPE_REPRESENTATION(#104,#12529);
#168=CONTEXT_DEPENDENT_SHAPE_REPRESENTATION(#105,#12530);
#169=CONTEXT_DEPENDENT_SHAPE_REPRESENTATION(#106,#12531);
#170=CONTEXT_DEPENDENT_SHAPE_REPRESENTATION(#107,#12532);
#171=CONTEXT_DEPENDENT_SHAPE_REPRESENTATION(#108,#12533);
#172=CONTEXT_DEPENDENT_SHAPE_REPRESENTATION(#109,#12534);
#173=CONTEXT_DEPENDENT_SHAPE_REPRESENTATION(#110,#12535);
#174=CONTEXT_DEPENDENT_SHAPE_REPRESENTATION(#111,#12536);
#175=CONTEXT_DEPENDENT_SHAPE_REPRESENTATION(#112,#12537);
#176=CONTEXT_DEPENDENT_SHAPE_REPRESENTATION(#113,#12538);
#177=CONTEXT_DEPENDENT_SHAPE_REPRESENTATION(#114,#12539);
#178=CONTEXT_DEPENDENT_SHAPE_REPRESENTATION(#115,#12540);
#179=CONTEXT_DEPENDENT_SHAPE_REPRESENTATION(#116,#12541);
#180=CONTEXT_DEPENDENT_SHAPE_REPRESENTATION(#117,#12542);
#181=CONTEXT_DEPENDENT_SHAPE_REPRESENTATION(#118,#12543);
#182=CONTEXT_DEPENDENT_SHAPE_REPRESENTATION(#119,#12544);
#183=CONTEXT_DEPENDENT_SHAPE_REPRESENTATION(#120,#12545);
#184=CONTEXT_DEPENDENT_SHAPE_REPRESENTATION(#121,#12546);
#185=CONTEXT_DEPENDENT_SHAPE_REPRESENTATION(#122,#12547);
#186=CONTEXT_DEPENDENT_SHAPE_REPRESENTATION(#123,#12548);
#187=CONTEXT_DEPENDENT_SHAPE_REPRESENTATION(#124,#12549);
#188=CONTEXT_DEPENDENT_SHAPE_REPRESENTATION(#125,#12550);
#189=CONTEXT_DEPENDENT_SHAPE_REPRESENTATION(#126,#12555);
#190=CONTEXT_DEPENDENT_SHAPE_REPRESENTATION(#127,#12556);
#191=CONTEXT_DEPENDENT_SHAPE_REPRESENTATION(#128,#12557);
#192=CONTEXT_DEPENDENT_SHAPE_REPRESENTATION(#129,#12563);
#193=CONTEXT_DEPENDENT_SHAPE_REPRESENTATION(#130,#12564);
#194=CONTEXT_DEPENDENT_SHAPE_REPRESENTATION(#131,#12565);
#195=CONTEXT_DEPENDENT_SHAPE_REPRESENTATION(#132,#12566);
#196=CONTEXT_DEPENDENT_SHAPE_REPRESENTATION(#133,#12567);
#197=CONTEXT_DEPENDENT_SHAPE_REPRESENTATION(#134,#12568);
#198=CONTEXT_DEPENDENT_SHAPE_REPRESENTATION(#135,#12569);
#199=CONTEXT_DEPENDENT_SHAPE_REPRESENTATION(#136,#12570);
#200=NEXT_ASSEMBLY_USAGE_OCCURRENCE('Inner ring:1','Inner ring:1',
'Inner ring:1',#12631,#12632,'Inner ring:1');
#201=NEXT_ASSEMBLY_USAGE_OCCURRENCE('Outer ring:1','Outer ring:1',
'Outer ring:1',#12631,#12633,'Outer ring:1');
#202=NEXT_ASSEMBLY_USAGE_OCCURRENCE('Balls:1','Balls:1','Balls:1',#12631,
#12634,'Balls:1');
#203=NEXT_ASSEMBLY_USAGE_OCCURRENCE('Cage:1','Cage:1','Cage:1',#12631,#12635,
'Cage:1');
#204=NEXT_ASSEMBLY_USAGE_OCCURRENCE('Seals 2RS:1','Seals 2RS:1',
'Seals 2RS:1',#12631,#12636,'Seals 2RS:1');
#205=NEXT_ASSEMBLY_USAGE_OCCURRENCE('Steel sleeve:1','Steel sleeve:1',
'Steel sleeve:1',#12637,#12638,'Steel sleeve:1');
#206=NEXT_ASSEMBLY_USAGE_OCCURRENCE('Ball retainer (plastic):1',
'Ball retainer (plastic):1','Ball retainer (plastic):1',#12637,#12639,
'Ball retainer (plastic):1');
#207=NEXT_ASSEMBLY_USAGE_OCCURRENCE('Base:1','Base:1','Base:1',#12618,#12619,
'Base:1');
#208=NEXT_ASSEMBLY_USAGE_OCCURRENCE('Foot strip:1','Foot strip:1',
'Foot strip:1',#12618,#12620,'Foot strip:1');
#209=NEXT_ASSEMBLY_USAGE_OCCURRENCE('Foot strip (1):1',
'Foot strip (1):1','Foot strip (1):1',#12618,#12621,'Foot strip (1):1');
#210=NEXT_ASSEMBLY_USAGE_OCCURRENCE('Bearing frame:1','Bearing frame:1',
'Bearing frame:1',#12618,#12622,'Bearing frame:1');
#211=NEXT_ASSEMBLY_USAGE_OCCURRENCE('Front bearing cap:1',
'Front bearing cap:1','Front bearing cap:1',#12618,#12623,
'Front bearing cap:1');
#212=NEXT_ASSEMBLY_USAGE_OCCURRENCE('Rear bearing cap:1',
'Rear bearing cap:1','Rear bearing cap:1',#12618,#12624,
'Rear bearing cap:1');
#213=NEXT_ASSEMBLY_USAGE_OCCURRENCE('Linear bearing cap:1',
'Linear bearing cap:1','Linear bearing cap:1',#12618,#12625,
'Linear bearing cap:1');
#214=NEXT_ASSEMBLY_USAGE_OCCURRENCE('Bar specimen envelope:1',
'Bar specimen envelope:1','Bar specimen envelope:1',#12618,#12626,
'Bar specimen envelope:1');
#215=NEXT_ASSEMBLY_USAGE_OCCURRENCE('Left bar guide:1',
'Left bar guide:1','Left bar guide:1',#12618,#12627,'Left bar guide:1');
#216=NEXT_ASSEMBLY_USAGE_OCCURRENCE('Right bar guide:1',
'Right bar guide:1','Right bar guide:1',#12618,#12628,
'Right bar guide:1');
#217=NEXT_ASSEMBLY_USAGE_OCCURRENCE('Closed lever stop:1',
'Closed lever stop:1','Closed lever stop:1',#12618,#12629,
'Closed lever stop:1');
#218=NEXT_ASSEMBLY_USAGE_OCCURRENCE('M5x14 Cap Screw:2',
'M5x14 Cap Screw:2','M5x14 Cap Screw:2',#12618,#12630,
'M5x14 Cap Screw:2');
#219=NEXT_ASSEMBLY_USAGE_OCCURRENCE('M5x14 Cap Screw:3',
'M5x14 Cap Screw:3','M5x14 Cap Screw:3',#12618,#12630,
'M5x14 Cap Screw:3');
#220=NEXT_ASSEMBLY_USAGE_OCCURRENCE('M5x14 Cap Screw:4',
'M5x14 Cap Screw:4','M5x14 Cap Screw:4',#12618,#12630,
'M5x14 Cap Screw:4');
#221=NEXT_ASSEMBLY_USAGE_OCCURRENCE('M5x14 Cap Screw:5',
'M5x14 Cap Screw:5','M5x14 Cap Screw:5',#12618,#12630,
'M5x14 Cap Screw:5');
#222=NEXT_ASSEMBLY_USAGE_OCCURRENCE(
'Sealed Ball Bearing - 10 x 30 x 9 mm:2',
'Sealed Ball Bearing - 10 x 30 x 9 mm:2',
'Sealed Ball Bearing - 10 x 30 x 9 mm:2',#12618,#12631,
'Sealed Ball Bearing - 10 x 30 x 9 mm:2');
#223=NEXT_ASSEMBLY_USAGE_OCCURRENCE(
'Linear Ball Bushing - 12 x 21 x 30 mm:2',
'Linear Ball Bushing - 12 x 21 x 30 mm:2',
'Linear Ball Bushing - 12 x 21 x 30 mm:2',#12618,#12637,
'Linear Ball Bushing - 12 x 21 x 30 mm:2');
#224=NEXT_ASSEMBLY_USAGE_OCCURRENCE('M4x10 Cap Screw:2',
'M4x10 Cap Screw:2','M4x10 Cap Screw:2',#12618,#12651,
'M4x10 Cap Screw:2');
#225=NEXT_ASSEMBLY_USAGE_OCCURRENCE('M4x10 Cap Screw:3',
'M4x10 Cap Screw:3','M4x10 Cap Screw:3',#12618,#12651,
'M4x10 Cap Screw:3');
#226=NEXT_ASSEMBLY_USAGE_OCCURRENCE('M4x10 Cap Screw:4',
'M4x10 Cap Screw:4','M4x10 Cap Screw:4',#12618,#12651,
'M4x10 Cap Screw:4');
#227=NEXT_ASSEMBLY_USAGE_OCCURRENCE('M4x10 Cap Screw:5',
'M4x10 Cap Screw:5','M4x10 Cap Screw:5',#12618,#12651,
'M4x10 Cap Screw:5');
#228=NEXT_ASSEMBLY_USAGE_OCCURRENCE('M4x10 Cap Screw:6',
'M4x10 Cap Screw:6','M4x10 Cap Screw:6',#12618,#12651,
'M4x10 Cap Screw:6');
#229=NEXT_ASSEMBLY_USAGE_OCCURRENCE('M4x10 Cap Screw:7',
'M4x10 Cap Screw:7','M4x10 Cap Screw:7',#12618,#12651,
'M4x10 Cap Screw:7');
#230=NEXT_ASSEMBLY_USAGE_OCCURRENCE('M4x10 Cap Screw:8',
'M4x10 Cap Screw:8','M4x10 Cap Screw:8',#12618,#12651,
'M4x10 Cap Screw:8');
#231=NEXT_ASSEMBLY_USAGE_OCCURRENCE('M4x10 Cap Screw:9',
'M4x10 Cap Screw:9','M4x10 Cap Screw:9',#12618,#12651,
'M4x10 Cap Screw:9');
#232=NEXT_ASSEMBLY_USAGE_OCCURRENCE('M4x10 Cap Screw:10',
'M4x10 Cap Screw:10','M4x10 Cap Screw:10',#12618,#12651,
'M4x10 Cap Screw:10');
#233=NEXT_ASSEMBLY_USAGE_OCCURRENCE('M4x10 Cap Screw:11',
'M4x10 Cap Screw:11','M4x10 Cap Screw:11',#12618,#12651,
'M4x10 Cap Screw:11');
#234=NEXT_ASSEMBLY_USAGE_OCCURRENCE('M4x10 Cap Screw:12',
'M4x10 Cap Screw:12','M4x10 Cap Screw:12',#12618,#12651,
'M4x10 Cap Screw:12');
#235=NEXT_ASSEMBLY_USAGE_OCCURRENCE('M4x10 Cap Screw:13',
'M4x10 Cap Screw:13','M4x10 Cap Screw:13',#12618,#12651,
'M4x10 Cap Screw:13');
#236=NEXT_ASSEMBLY_USAGE_OCCURRENCE('Cap Screw - M4x16:3',
'Cap Screw - M4x16:3','Cap Screw - M4x16:3',#12618,#12652,
'Cap Screw - M4x16:3');
#237=NEXT_ASSEMBLY_USAGE_OCCURRENCE('Cap Screw - M4x16:4',
'Cap Screw - M4x16:4','Cap Screw - M4x16:4',#12618,#12652,
'Cap Screw - M4x16:4');
#238=NEXT_ASSEMBLY_USAGE_OCCURRENCE('Cap Screw - M4x16:5',
'Cap Screw - M4x16:5','Cap Screw - M4x16:5',#12618,#12652,
'Cap Screw - M4x16:5');
#239=NEXT_ASSEMBLY_USAGE_OCCURRENCE('Cap Screw - M4x16:6',
'Cap Screw - M4x16:6','Cap Screw - M4x16:6',#12618,#12652,
'Cap Screw - M4x16:6');
#240=NEXT_ASSEMBLY_USAGE_OCCURRENCE('M4x30 stop screw:2',
'M4x30 stop screw:2','M4x30 stop screw:2',#12618,#12640,
'M4x30 stop screw:2');
#241=NEXT_ASSEMBLY_USAGE_OCCURRENCE('Lever and spindle:1',
'Lever and spindle:1','Lever and spindle:1',#12641,#12642,
'Lever and spindle:1');
#242=NEXT_ASSEMBLY_USAGE_OCCURRENCE('Inner race spacer:1',
'Inner race spacer:1','Inner race spacer:1',#12641,#12643,
'Inner race spacer:1');
#243=NEXT_ASSEMBLY_USAGE_OCCURRENCE('Shaft collar:1','Shaft collar:1',
'Shaft collar:1',#12641,#12644,'Shaft collar:1');
#244=NEXT_ASSEMBLY_USAGE_OCCURRENCE('Lever link pin:1',
'Lever link pin:1','Lever link pin:1',#12641,#12645,'Lever link pin:1');
#245=NEXT_ASSEMBLY_USAGE_OCCURRENCE('Rear pin spacer:1',
'Rear pin spacer:1','Rear pin spacer:1',#12641,#12646,
'Rear pin spacer:1');
#246=NEXT_ASSEMBLY_USAGE_OCCURRENCE('Front pin spacer:1',
'Front pin spacer:1','Front pin spacer:1',#12641,#12647,
'Front pin spacer:1');
#247=NEXT_ASSEMBLY_USAGE_OCCURRENCE('Front pin keeper:1',
'Front pin keeper:1','Front pin keeper:1',#12641,#12648,
'Front pin keeper:1');
#248=NEXT_ASSEMBLY_USAGE_OCCURRENCE('Rear pin keeper:1',
'Rear pin keeper:1','Rear pin keeper:1',#12641,#12649,
'Rear pin keeper:1');
#249=NEXT_ASSEMBLY_USAGE_OCCURRENCE('M4x4 collar screw:2',
'M4x4 collar screw:2','M4x4 collar screw:2',#12641,#12650,
'M4x4 collar screw:2');
#250=NEXT_ASSEMBLY_USAGE_OCCURRENCE('M4x10 Cap Screw:14',
'M4x10 Cap Screw:14','M4x10 Cap Screw:14',#12641,#12651,
'M4x10 Cap Screw:14');
#251=NEXT_ASSEMBLY_USAGE_OCCURRENCE('Cap Screw - M4x16:2',
'Cap Screw - M4x16:2','Cap Screw - M4x16:2',#12641,#12652,
'Cap Screw - M4x16:2');
#252=NEXT_ASSEMBLY_USAGE_OCCURRENCE('Connecting link:1',
'Connecting link:1','Connecting link:1',#12653,#12654,
'Connecting link:1');
#253=NEXT_ASSEMBLY_USAGE_OCCURRENCE('Link bush:1','Link bush:1',
'Link bush:1',#12653,#12655,'Link bush:1');
#254=NEXT_ASSEMBLY_USAGE_OCCURRENCE('Link bush (1):1','Link bush (1):1',
'Link bush (1):1',#12653,#12656,'Link bush (1):1');
#255=NEXT_ASSEMBLY_USAGE_OCCURRENCE('Plunger and fork:1',
'Plunger and fork:1','Plunger and fork:1',#12657,#12658,
'Plunger and fork:1');
#256=NEXT_ASSEMBLY_USAGE_OCCURRENCE('Fork pin:1','Fork pin:1',
'Fork pin:1',#12657,#12659,'Fork pin:1');
#257=NEXT_ASSEMBLY_USAGE_OCCURRENCE(
'Elastomer pressure pad installed:1',
'Elastomer pressure pad installed:1',
'Elastomer pressure pad installed:1',#12657,#12660,
'Elastomer pressure pad installed:1');
#258=NEXT_ASSEMBLY_USAGE_OCCURRENCE('Socket Set Screw - M4x6:2',
'Socket Set Screw - M4x6:2','Socket Set Screw - M4x6:2',#12657,#12661,
'Socket Set Screw - M4x6:2');
#259=NEXT_ASSEMBLY_USAGE_OCCURRENCE('Base and guide:1',
'Base and guide:1','Base and guide:1',#12617,#12618,'Base and guide:1');
#260=NEXT_ASSEMBLY_USAGE_OCCURRENCE('Operating lever:1',
'Operating lever:1','Operating lever:1',#12617,#12641,
'Operating lever:1');
#261=NEXT_ASSEMBLY_USAGE_OCCURRENCE('Connecting link (1):1',
'Connecting link (1):1','Connecting link (1):1',#12617,#12653,
'Connecting link (1):1');
#262=NEXT_ASSEMBLY_USAGE_OCCURRENCE('Pressure plunger:1',
'Pressure plunger:1','Pressure plunger:1',#12617,#12657,
'Pressure plunger:1');
#263=B_SPLINE_CURVE_WITH_KNOTS('',3,(#10837,#10838,#10839,#10840,#10841,
#10842,#10843,#10844,#10845,#10846,#10847,#10848,#10849,#10850,#10851,#10852,
#10853,#10854,#10855,#10856,#10857,#10858),.UNSPECIFIED.,.F.,.F.,(4,2,2,
2,2,2,2,2,2,2,4),(0.0473477652366656,0.126350602536658,0.189525903804987,
0.252701205073317,0.313298422430275,0.373895639787233,0.434492857144191,
0.495090074501149,0.558265375769478,0.621440677037807,0.7004435143378),
 .UNSPECIFIED.);
#264=B_SPLINE_CURVE_WITH_KNOTS('',3,(#10862,#10863,#10864,#10865,#10866,
#10867,#10868,#10869,#10870,#10871,#10872,#10873,#10874,#10875,#10876,#10877,
#10878,#10879,#10880,#10881,#10882,#10883),.UNSPECIFIED.,.F.,.F.,(4,2,2,
2,2,2,2,2,2,2,4),(0.0464897534940957,0.0852567806515119,0.170513561303024,
0.246687263103517,0.308657850341199,0.370628437578881,0.432599024816563,
0.494569612054245,0.570743313854739,0.656000094506251,0.694767121663666),
 .UNSPECIFIED.);
#265=B_SPLINE_CURVE_WITH_KNOTS('',3,(#10889,#10890,#10891,#10892,#10893,
#10894,#10895,#10896,#10897,#10898,#10899,#10900,#10901,#10902,#10903,#10904,
#10905,#10906,#10907,#10908,#10909,#10910),.UNSPECIFIED.,.F.,.F.,(4,2,2,
2,2,2,2,2,2,2,4),(0.0464897534940957,0.0852567806515118,0.170513561303024,
0.246687263103517,0.308657850341199,0.370628437578881,0.432599024816563,
0.494569612054245,0.570743313854738,0.65600009450625,0.694767121663666),
 .UNSPECIFIED.);
#266=B_SPLINE_CURVE_WITH_KNOTS('',3,(#10914,#10915,#10916,#10917,#10918,
#10919,#10920,#10921,#10922,#10923,#10924,#10925,#10926,#10927,#10928,#10929,
#10930,#10931,#10932,#10933,#10934,#10935),.UNSPECIFIED.,.F.,.F.,(4,2,2,
2,2,2,2,2,2,2,4),(0.0464897534940957,0.0852567806515119,0.170513561303024,
0.246687263103517,0.308657850341199,0.370628437578881,0.432599024816563,
0.494569612054245,0.570743313854739,0.656000094506251,0.694767121663666),
 .UNSPECIFIED.);
#267=B_SPLINE_CURVE_WITH_KNOTS('',3,(#10939,#10940,#10941,#10942,#10943,
#10944,#10945,#10946,#10947,#10948,#10949,#10950),.UNSPECIFIED.,.F.,.F.,
(4,2,2,2,2,4),(0.0464897534940957,0.0852567806515119,0.170513561303024,
0.246687263103517,0.308657850341199,0.370628437578881),.UNSPECIFIED.);
#268=B_SPLINE_CURVE_WITH_KNOTS('',3,(#10955,#10956,#10957,#10958,#10959,
#10960,#10961,#10962,#10963,#10964,#10965,#10966),.UNSPECIFIED.,.F.,.F.,
(4,2,2,2,2,4),(0.370628437578881,0.432599024816563,0.494569612054245,0.570743313854738,
0.65600009450625,0.694767121663666),.UNSPECIFIED.);
#269=B_SPLINE_CURVE_WITH_KNOTS('',3,(#10970,#10971,#10972,#10973,#10974,
#10975,#10976,#10977,#10978,#10979,#10980,#10981,#10982,#10983,#10984,#10985,
#10986,#10987,#10988,#10989,#10990,#10991),.UNSPECIFIED.,.F.,.F.,(4,2,2,
2,2,2,2,2,2,2,4),(0.0464897534940957,0.0852567806515121,0.170513561303024,
0.246687263103518,0.308657850341199,0.370628437578881,0.432599024816563,
0.494569612054245,0.570743313854738,0.65600009450625,0.694767121663666),
 .UNSPECIFIED.);
#270=B_SPLINE_CURVE_WITH_KNOTS('',3,(#10995,#10996,#10997,#10998,#10999,
#11000,#11001,#11002,#11003,#11004,#11005,#11006,#11007,#11008,#11009,#11010,
#11011,#11012,#11013,#11014,#11015,#11016),.UNSPECIFIED.,.F.,.F.,(4,2,2,
2,2,2,2,2,2,2,4),(0.0464897534940957,0.0852567806515119,0.170513561303024,
0.246687263103517,0.308657850341199,0.370628437578881,0.432599024816563,
0.494569612054245,0.570743313854738,0.65600009450625,0.694767121663667),
 .UNSPECIFIED.);
#271=B_SPLINE_CURVE_WITH_KNOTS('',3,(#11020,#11021,#11022,#11023,#11024,
#11025,#11026,#11027,#11028,#11029,#11030,#11031,#11032,#11033,#11034,#11035,
#11036,#11037,#11038,#11039,#11040,#11041),.UNSPECIFIED.,.F.,.F.,(4,2,2,
2,2,2,2,2,2,2,4),(0.0464897534940957,0.0852567806515119,0.170513561303024,
0.246687263103517,0.308657850341199,0.370628437578881,0.432599024816563,
0.494569612054245,0.570743313854738,0.65600009450625,0.694767121663666),
 .UNSPECIFIED.);
#272=B_SPLINE_CURVE_WITH_KNOTS('',3,(#11045,#11046,#11047,#11048,#11049,
#11050,#11051,#11052,#11053,#11054,#11055,#11056,#11057,#11058,#11059,#11060,
#11061,#11062,#11063,#11064,#11065,#11066),.UNSPECIFIED.,.F.,.F.,(4,2,2,
2,2,2,2,2,2,2,4),(0.0464897534940957,0.0852567806515119,0.170513561303024,
0.246687263103517,0.308657850341199,0.370628437578881,0.432599024816563,
0.494569612054245,0.570743313854739,0.656000094506251,0.694767121663667),
 .UNSPECIFIED.);
#273=B_SPLINE_CURVE_WITH_KNOTS('',3,(#11074,#11075,#11076,#11077,#11078,
#11079,#11080,#11081,#11082,#11083,#11084,#11085,#11086,#11087,#11088,#11089,
#11090,#11091,#11092,#11093,#11094,#11095),.UNSPECIFIED.,.F.,.F.,(4,2,2,
2,2,2,2,2,2,2,4),(0.0473477652366656,0.126350602536658,0.189525903804987,
0.252701205073316,0.313298422430274,0.373895639787232,0.434492857144191,
0.495090074501149,0.558265375769478,0.621440677037807,0.7004435143378),
 .UNSPECIFIED.);
#274=B_SPLINE_CURVE_WITH_KNOTS('',3,(#11103,#11104,#11105,#11106,#11107,
#11108,#11109,#11110,#11111,#11112,#11113,#11114,#11115,#11116,#11117,#11118,
#11119,#11120,#11121,#11122,#11123,#11124),.UNSPECIFIED.,.F.,.F.,(4,2,2,
2,2,2,2,2,2,2,4),(0.0473477652366656,0.126350602536658,0.189525903804987,
0.252701205073317,0.313298422430275,0.373895639787233,0.434492857144191,
0.495090074501149,0.558265375769478,0.621440677037807,0.7004435143378),
 .UNSPECIFIED.);
#275=B_SPLINE_CURVE_WITH_KNOTS('',3,(#11133,#11134,#11135,#11136,#11137,
#11138,#11139,#11140,#11141,#11142,#11143,#11144),.UNSPECIFIED.,.F.,.F.,
(4,2,2,2,2,4),(0.0473477652366656,0.126350602536658,0.189525903804987,0.252701205073316,
0.313298422430275,0.373895639787233),.UNSPECIFIED.);
#276=B_SPLINE_CURVE_WITH_KNOTS('',3,(#11146,#11147,#11148,#11149,#11150,
#11151,#11152,#11153,#11154,#11155,#11156,#11157),.UNSPECIFIED.,.F.,.F.,
(4,2,2,2,2,4),(0.373895639787233,0.434492857144191,0.495090074501149,0.558265375769478,
0.621440677037807,0.7004435143378),.UNSPECIFIED.);
#277=B_SPLINE_CURVE_WITH_KNOTS('',3,(#11164,#11165,#11166,#11167,#11168,
#11169,#11170,#11171,#11172,#11173,#11174,#11175,#11176,#11177,#11178,#11179,
#11180,#11181,#11182,#11183,#11184,#11185),.UNSPECIFIED.,.F.,.F.,(4,2,2,
2,2,2,2,2,2,2,4),(0.0473477652366656,0.126350602536658,0.189525903804987,
0.252701205073316,0.313298422430275,0.373895639787233,0.434492857144191,
0.495090074501149,0.558265375769478,0.621440677037807,0.7004435143378),
 .UNSPECIFIED.);
#278=B_SPLINE_CURVE_WITH_KNOTS('',3,(#11193,#11194,#11195,#11196,#11197,
#11198,#11199,#11200,#11201,#11202,#11203,#11204,#11205,#11206,#11207,#11208,
#11209,#11210,#11211,#11212,#11213,#11214),.UNSPECIFIED.,.F.,.F.,(4,2,2,
2,2,2,2,2,2,2,4),(0.0473477652366656,0.126350602536658,0.189525903804987,
0.252701205073317,0.313298422430275,0.373895639787233,0.434492857144191,
0.495090074501149,0.558265375769478,0.621440677037807,0.7004435143378),
 .UNSPECIFIED.);
#279=B_SPLINE_CURVE_WITH_KNOTS('',3,(#11222,#11223,#11224,#11225,#11226,
#11227,#11228,#11229,#11230,#11231,#11232,#11233,#11234,#11235,#11236,#11237,
#11238,#11239,#11240,#11241,#11242,#11243),.UNSPECIFIED.,.F.,.F.,(4,2,2,
2,2,2,2,2,2,2,4),(0.0473477652366656,0.126350602536658,0.189525903804987,
0.252701205073316,0.313298422430275,0.373895639787233,0.434492857144191,
0.495090074501149,0.558265375769478,0.621440677037807,0.7004435143378),
 .UNSPECIFIED.);
#280=B_SPLINE_CURVE_WITH_KNOTS('',3,(#11252,#11253,#11254,#11255,#11256,
#11257,#11258,#11259,#11260,#11261,#11262,#11263,#11264,#11265,#11266,#11267,
#11268,#11269,#11270,#11271,#11272,#11273),.UNSPECIFIED.,.F.,.F.,(4,2,2,
2,2,2,2,2,2,2,4),(0.0473477652366656,0.126350602536658,0.189525903804987,
0.252701205073317,0.313298422430275,0.373895639787233,0.434492857144191,
0.495090074501149,0.558265375769478,0.621440677037807,0.7004435143378),
 .UNSPECIFIED.);
#281=B_SPLINE_CURVE_WITH_KNOTS('',3,(#11610,#11611,#11612,#11613,#11614,
#11615,#11616,#11617,#11618,#11619,#11620,#11621,#11622,#11623),
 .UNSPECIFIED.,.F.,.F.,(4,2,2,2,2,2,4),(0.618551524396288,0.626563103102763,
0.689203386094986,0.751843669087208,0.814483952079431,0.877124235071654,
0.88513581377813),.UNSPECIFIED.);
#282=B_SPLINE_CURVE_WITH_KNOTS('',3,(#11629,#11630,#11631,#11632,#11633,
#11634,#11635,#11636,#11637,#11638,#11639,#11640,#11641,#11642,#11643,#11644,
#11645,#11646),.UNSPECIFIED.,.F.,.F.,(4,2,2,2,2,2,2,2,4),(0.,0.0623062782223138,
0.124612556444628,0.186916384615148,0.249220212785668,0.311524040956189,
0.373827869126709,0.436134147349023,0.498440425571337),.UNSPECIFIED.);
#283=B_SPLINE_CURVE_WITH_KNOTS('',3,(#11647,#11648,#11649,#11650,#11651,
#11652,#11653,#11654,#11655,#11656,#11657,#11658,#11659,#11660,#11661,#11662,
#11663,#11664),.UNSPECIFIED.,.F.,.F.,(4,2,2,2,2,2,2,2,4),(0.498440425571337,
0.560746703793651,0.623052982015964,0.685356810186485,0.747660638357005,
0.809964466527525,0.872268294698046,0.93457457292036,0.996880851142673),
 .UNSPECIFIED.);
#284=B_SPLINE_CURVE_WITH_KNOTS('',3,(#11667,#11668,#11669,#11670,#11671,
#11672,#11673,#11674,#11675,#11676,#11677,#11678,#11679,#11680),
 .UNSPECIFIED.,.F.,.F.,(4,2,2,2,2,2,4),(0.117322411671483,0.125333990377957,
0.18797427337018,0.250614556362403,0.313254839354626,0.375895122346849,
0.383906701053325),.UNSPECIFIED.);
#285=B_SPLINE_CURVE_WITH_KNOTS('',3,(#12174,#12175,#12176,#12177,#12178,
#12179,#12180,#12181,#12182,#12183),.UNSPECIFIED.,.F.,.F.,(4,2,2,2,4),(0.66642709076087,
0.700624974512804,0.764181514210609,0.827738053908413,0.861935937660348),
 .UNSPECIFIED.);
#286=B_SPLINE_CURVE_WITH_KNOTS('',3,(#12191,#12192,#12193,#12194,#12195,
#12196,#12197,#12198,#12199,#12200),.UNSPECIFIED.,.F.,.F.,(4,2,2,2,4),(0.156972747953797,
0.191170631705732,0.254727171403536,0.318283711101341,0.352481594853276),
 .UNSPECIFIED.);
#287=SPHERICAL_SURFACE('',#7369,0.23815);
#288=SPHERICAL_SURFACE('',#7371,0.23815);
#289=SPHERICAL_SURFACE('',#7373,0.23815);
#290=SPHERICAL_SURFACE('',#7375,0.23815);
#291=SPHERICAL_SURFACE('',#7377,0.23815);
#292=SPHERICAL_SURFACE('',#7379,0.23815);
#293=SPHERICAL_SURFACE('',#7381,0.23815);
#294=SPHERICAL_SURFACE('',#7383,0.23815);
#295=SPHERICAL_SURFACE('',#7386,0.247676);
#296=SPHERICAL_SURFACE('',#7402,0.247676);
#297=SPHERICAL_SURFACE('',#7407,0.247676);
#298=SPHERICAL_SURFACE('',#7412,0.247676);
#299=SPHERICAL_SURFACE('',#7417,0.247676);
#300=SPHERICAL_SURFACE('',#7422,0.247676);
#301=SPHERICAL_SURFACE('',#7427,0.247676);
#302=SPHERICAL_SURFACE('',#7435,0.247676);
#303=TOROIDAL_SURFACE('',#7329,1.,0.247676);
#304=TOROIDAL_SURFACE('',#7349,1.,0.247676);
#305=CONICAL_SURFACE('',#7316,0.4,0.785398163397448);
#306=CONICAL_SURFACE('',#7320,0.41,0.785398163397448);
#307=CONICAL_SURFACE('',#7324,0.26,0.463647609000806);
#308=CONICAL_SURFACE('',#7340,0.53,0.785398163397448);
#309=CONICAL_SURFACE('',#7347,0.53,0.785398163397448);
#310=CONICAL_SURFACE('',#7360,1.47,0.785398163397449);
#311=CONICAL_SURFACE('',#7364,1.47,0.785398163397449);
#312=CONICAL_SURFACE('',#7530,0.325,0.785398163397448);
#313=CONICAL_SURFACE('',#7534,0.335,0.785398163397448);
#314=CONICAL_SURFACE('',#7538,0.21,0.463647609000806);
#315=CONICAL_SURFACE('',#7542,0.18,0.785398163397448);
#316=CONICAL_SURFACE('',#7675,0.185,0.785398163397449);
#317=CONICAL_SURFACE('',#7691,0.325,0.785398163397448);
#318=CONICAL_SURFACE('',#7695,0.335,0.785398163397448);
#319=CONICAL_SURFACE('',#7699,0.21,0.463647609000806);
#320=CONICAL_SURFACE('',#7705,0.325,0.785398163397448);
#321=CONICAL_SURFACE('',#7709,0.335,0.785398163397448);
#322=CONICAL_SURFACE('',#7713,0.21,0.463647609000806);
#323=CONICAL_SURFACE('',#7717,0.18,0.785398163397448);
#324=CONICAL_SURFACE('',#7879,0.185,0.785398163397449);
#325=CONICAL_SURFACE('',#7883,0.1625,0.785398163397449);
#326=ORIENTED_CLOSED_SHELL('',*,#6580,.F.);
#327=ORIENTED_CLOSED_SHELL('',*,#6597,.F.);
#328=ORIENTED_CLOSED_SHELL('',*,#6608,.F.);
#329=ORIENTED_CLOSED_SHELL('',*,#6611,.F.);
#330=BREP_WITH_VOIDS('Body1',#6581,(#326));
#331=BREP_WITH_VOIDS('Body1',#6598,(#327));
#332=BREP_WITH_VOIDS('Body1',#6609,(#328));
#333=BREP_WITH_VOIDS('Body1',#6610,(#329));
#334=SHAPE_REPRESENTATION_RELATIONSHIP('SRR','None',#12573,#372);
#335=SHAPE_REPRESENTATION_RELATIONSHIP('SRR','None',#12574,#373);
#336=SHAPE_REPRESENTATION_RELATIONSHIP('SRR','None',#12575,#374);
#337=SHAPE_REPRESENTATION_RELATIONSHIP('SRR','None',#12576,#375);
#338=SHAPE_REPRESENTATION_RELATIONSHIP('SRR','None',#12577,#376);
#339=SHAPE_REPRESENTATION_RELATIONSHIP('SRR','None',#12578,#377);
#340=SHAPE_REPRESENTATION_RELATIONSHIP('SRR','None',#12579,#378);
#341=SHAPE_REPRESENTATION_RELATIONSHIP('SRR','None',#12580,#379);
#342=SHAPE_REPRESENTATION_RELATIONSHIP('SRR','None',#12581,#380);
#343=SHAPE_REPRESENTATION_RELATIONSHIP('SRR','None',#12582,#381);
#344=SHAPE_REPRESENTATION_RELATIONSHIP('SRR','None',#12583,#382);
#345=SHAPE_REPRESENTATION_RELATIONSHIP('SRR','None',#12584,#383);
#346=SHAPE_REPRESENTATION_RELATIONSHIP('SRR','None',#12586,#384);
#347=SHAPE_REPRESENTATION_RELATIONSHIP('SRR','None',#12587,#385);
#348=SHAPE_REPRESENTATION_RELATIONSHIP('SRR','None',#12588,#386);
#349=SHAPE_REPRESENTATION_RELATIONSHIP('SRR','None',#12589,#387);
#350=SHAPE_REPRESENTATION_RELATIONSHIP('SRR','None',#12590,#388);
#351=SHAPE_REPRESENTATION_RELATIONSHIP('SRR','None',#12592,#389);
#352=SHAPE_REPRESENTATION_RELATIONSHIP('SRR','None',#12593,#390);
#353=SHAPE_REPRESENTATION_RELATIONSHIP('SRR','None',#12594,#391);
#354=SHAPE_REPRESENTATION_RELATIONSHIP('SRR','None',#12596,#392);
#355=SHAPE_REPRESENTATION_RELATIONSHIP('SRR','None',#12597,#393);
#356=SHAPE_REPRESENTATION_RELATIONSHIP('SRR','None',#12598,#394);
#357=SHAPE_REPRESENTATION_RELATIONSHIP('SRR','None',#12599,#395);
#358=SHAPE_REPRESENTATION_RELATIONSHIP('SRR','None',#12600,#396);
#359=SHAPE_REPRESENTATION_RELATIONSHIP('SRR','None',#12601,#397);
#360=SHAPE_REPRESENTATION_RELATIONSHIP('SRR','None',#12602,#398);
#361=SHAPE_REPRESENTATION_RELATIONSHIP('SRR','None',#12603,#399);
#362=SHAPE_REPRESENTATION_RELATIONSHIP('SRR','None',#12604,#400);
#363=SHAPE_REPRESENTATION_RELATIONSHIP('SRR','None',#12605,#401);
#364=SHAPE_REPRESENTATION_RELATIONSHIP('SRR','None',#12606,#402);
#365=SHAPE_REPRESENTATION_RELATIONSHIP('SRR','None',#12608,#403);
#366=SHAPE_REPRESENTATION_RELATIONSHIP('SRR','None',#12609,#404);
#367=SHAPE_REPRESENTATION_RELATIONSHIP('SRR','None',#12610,#405);
#368=SHAPE_REPRESENTATION_RELATIONSHIP('SRR','None',#12612,#406);
#369=SHAPE_REPRESENTATION_RELATIONSHIP('SRR','None',#12613,#407);
#370=SHAPE_REPRESENTATION_RELATIONSHIP('SRR','None',#12614,#408);
#371=SHAPE_REPRESENTATION_RELATIONSHIP('SRR','None',#12615,#409);
#372=ADVANCED_BREP_SHAPE_REPRESENTATION('',(#457),#12370);
#373=ADVANCED_BREP_SHAPE_REPRESENTATION('',(#458),#12371);
#374=ADVANCED_BREP_SHAPE_REPRESENTATION('',(#459),#12372);
#375=ADVANCED_BREP_SHAPE_REPRESENTATION('',(#460),#12373);
#376=ADVANCED_BREP_SHAPE_REPRESENTATION('',(#461),#12374);
#377=ADVANCED_BREP_SHAPE_REPRESENTATION('',(#462),#12375);
#378=ADVANCED_BREP_SHAPE_REPRESENTATION('',(#463),#12376);
#379=ADVANCED_BREP_SHAPE_REPRESENTATION('',(#464),#12377);
#380=ADVANCED_BREP_SHAPE_REPRESENTATION('',(#465),#12378);
#381=ADVANCED_BREP_SHAPE_REPRESENTATION('',(#466),#12379);
#382=ADVANCED_BREP_SHAPE_REPRESENTATION('',(#467),#12380);
#383=ADVANCED_BREP_SHAPE_REPRESENTATION('',(#330),#12381);
#384=ADVANCED_BREP_SHAPE_REPRESENTATION('',(#468),#12383);
#385=ADVANCED_BREP_SHAPE_REPRESENTATION('',(#469),#12384);
#386=ADVANCED_BREP_SHAPE_REPRESENTATION('',(#470,#471,#472,#473,#474,#475,
#476,#477),#12385);
#387=ADVANCED_BREP_SHAPE_REPRESENTATION('',(#478),#12386);
#388=ADVANCED_BREP_SHAPE_REPRESENTATION('',(#479,#480),#12387);
#389=ADVANCED_BREP_SHAPE_REPRESENTATION('',(#481),#12389);
#390=ADVANCED_BREP_SHAPE_REPRESENTATION('',(#482),#12390);
#391=ADVANCED_BREP_SHAPE_REPRESENTATION('',(#331),#12391);
#392=ADVANCED_BREP_SHAPE_REPRESENTATION('',(#483),#12393);
#393=ADVANCED_BREP_SHAPE_REPRESENTATION('',(#484),#12394);
#394=ADVANCED_BREP_SHAPE_REPRESENTATION('',(#485),#12395);
#395=ADVANCED_BREP_SHAPE_REPRESENTATION('',(#486),#12396);
#396=ADVANCED_BREP_SHAPE_REPRESENTATION('',(#487),#12397);
#397=ADVANCED_BREP_SHAPE_REPRESENTATION('',(#488),#12398);
#398=ADVANCED_BREP_SHAPE_REPRESENTATION('',(#489),#12399);
#399=ADVANCED_BREP_SHAPE_REPRESENTATION('',(#490),#12400);
#400=ADVANCED_BREP_SHAPE_REPRESENTATION('',(#491),#12401);
#401=ADVANCED_BREP_SHAPE_REPRESENTATION('',(#332),#12402);
#402=ADVANCED_BREP_SHAPE_REPRESENTATION('',(#333),#12403);
#403=ADVANCED_BREP_SHAPE_REPRESENTATION('',(#492),#12405);
#404=ADVANCED_BREP_SHAPE_REPRESENTATION('',(#493),#12406);
#405=ADVANCED_BREP_SHAPE_REPRESENTATION('',(#494),#12407);
#406=ADVANCED_BREP_SHAPE_REPRESENTATION('',(#495,#496),#12409);
#407=ADVANCED_BREP_SHAPE_REPRESENTATION('',(#497),#12410);
#408=ADVANCED_BREP_SHAPE_REPRESENTATION('',(#498),#12411);
#409=ADVANCED_BREP_SHAPE_REPRESENTATION('',(#499),#12412);
#410=STYLED_ITEM('',(#12848),#457);
#411=STYLED_ITEM('',(#12855),#458);
#412=STYLED_ITEM('',(#12855),#459);
#413=STYLED_ITEM('',(#12869),#460);
#414=STYLED_ITEM('',(#12869),#461);
#415=STYLED_ITEM('',(#12869),#462);
#416=STYLED_ITEM('',(#12869),#463);
#417=STYLED_ITEM('',(#12883),#464);
#418=STYLED_ITEM('',(#12862),#465);
#419=STYLED_ITEM('',(#12883),#466);
#420=STYLED_ITEM('',(#12862),#467);
#421=STYLED_ITEM('',(#12876),#330);
#422=STYLED_ITEM('',(#12869),#468);
#423=STYLED_ITEM('',(#12869),#469);
#424=STYLED_ITEM('',(#12869),#470);
#425=STYLED_ITEM('',(#12869),#471);
#426=STYLED_ITEM('',(#12869),#472);
#427=STYLED_ITEM('',(#12869),#473);
#428=STYLED_ITEM('',(#12869),#474);
#429=STYLED_ITEM('',(#12869),#475);
#430=STYLED_ITEM('',(#12869),#476);
#431=STYLED_ITEM('',(#12869),#477);
#432=STYLED_ITEM('',(#12869),#478);
#433=STYLED_ITEM('',(#12869),#479);
#434=STYLED_ITEM('',(#12869),#480);
#435=STYLED_ITEM('',(#12883),#481);
#436=STYLED_ITEM('',(#12862),#482);
#437=STYLED_ITEM('',(#12876),#331);
#438=STYLED_ITEM('',(#12862),#483);
#439=STYLED_ITEM('',(#12869),#484);
#440=STYLED_ITEM('',(#12869),#485);
#441=STYLED_ITEM('',(#12869),#486);
#442=STYLED_ITEM('',(#12869),#487);
#443=STYLED_ITEM('',(#12869),#488);
#444=STYLED_ITEM('',(#12869),#489);
#445=STYLED_ITEM('',(#12869),#490);
#446=STYLED_ITEM('',(#12876),#491);
#447=STYLED_ITEM('',(#12876),#332);
#448=STYLED_ITEM('',(#12876),#333);
#449=STYLED_ITEM('',(#12862),#492);
#450=STYLED_ITEM('',(#12883),#493);
#451=STYLED_ITEM('',(#12883),#494);
#452=STYLED_ITEM('',(#12883),#495);
#453=STYLED_ITEM('',(#12883),#496);
#454=STYLED_ITEM('',(#12869),#497);
#455=STYLED_ITEM('',(#12883),#498);
#456=STYLED_ITEM('',(#12876),#499);
#457=MANIFOLD_SOLID_BREP('Body1',#6569);
#458=MANIFOLD_SOLID_BREP('Body1',#6570);
#459=MANIFOLD_SOLID_BREP('Body1',#6571);
#460=MANIFOLD_SOLID_BREP('Body1',#6572);
#461=MANIFOLD_SOLID_BREP('Body1',#6573);
#462=MANIFOLD_SOLID_BREP('Body1',#6574);
#463=MANIFOLD_SOLID_BREP('Body1',#6575);
#464=MANIFOLD_SOLID_BREP('Body1',#6576);
#465=MANIFOLD_SOLID_BREP('Body1',#6577);
#466=MANIFOLD_SOLID_BREP('Body1',#6578);
#467=MANIFOLD_SOLID_BREP('Body1',#6579);
#468=MANIFOLD_SOLID_BREP('Body1',#6582);
#469=MANIFOLD_SOLID_BREP('Body1',#6583);
#470=MANIFOLD_SOLID_BREP('Body1',#6584);
#471=MANIFOLD_SOLID_BREP('Body2',#6585);
#472=MANIFOLD_SOLID_BREP('Body3',#6586);
#473=MANIFOLD_SOLID_BREP('Body4',#6587);
#474=MANIFOLD_SOLID_BREP('Body5',#6588);
#475=MANIFOLD_SOLID_BREP('Body6',#6589);
#476=MANIFOLD_SOLID_BREP('Body7',#6590);
#477=MANIFOLD_SOLID_BREP('Body8',#6591);
#478=MANIFOLD_SOLID_BREP('Continuous crown cage',#6592);
#479=MANIFOLD_SOLID_BREP('Body1',#6593);
#480=MANIFOLD_SOLID_BREP('Body2',#6594);
#481=MANIFOLD_SOLID_BREP('Body1',#6595);
#482=MANIFOLD_SOLID_BREP('Body1',#6596);
#483=MANIFOLD_SOLID_BREP('Body1',#6599);
#484=MANIFOLD_SOLID_BREP('Body1',#6600);
#485=MANIFOLD_SOLID_BREP('Body1',#6601);
#486=MANIFOLD_SOLID_BREP('Body1',#6602);
#487=MANIFOLD_SOLID_BREP('Body1',#6603);
#488=MANIFOLD_SOLID_BREP('Body1',#6604);
#489=MANIFOLD_SOLID_BREP('Body1',#6605);
#490=MANIFOLD_SOLID_BREP('Body1',#6606);
#491=MANIFOLD_SOLID_BREP('Body1',#6607);
#492=MANIFOLD_SOLID_BREP('Body1',#6612);
#493=MANIFOLD_SOLID_BREP('Body1',#6613);
#494=MANIFOLD_SOLID_BREP('Body1',#6614);
#495=MANIFOLD_SOLID_BREP('Body1',#6615);
#496=MANIFOLD_SOLID_BREP('Body2',#6616);
#497=MANIFOLD_SOLID_BREP('Body1',#6617);
#498=MANIFOLD_SOLID_BREP('Body1',#6618);
#499=MANIFOLD_SOLID_BREP('Body1',#6619);
#500=FACE_BOUND('',#1307,.T.);
#501=FACE_BOUND('',#1308,.T.);
#502=FACE_BOUND('',#1309,.T.);
#503=FACE_BOUND('',#1310,.T.);
#504=FACE_BOUND('',#1311,.T.);
#505=FACE_BOUND('',#1312,.T.);
#506=FACE_BOUND('',#1313,.T.);
#507=FACE_BOUND('',#1314,.T.);
#508=FACE_BOUND('',#1316,.T.);
#509=FACE_BOUND('',#1317,.T.);
#510=FACE_BOUND('',#1318,.T.);
#511=FACE_BOUND('',#1319,.T.);
#512=FACE_BOUND('',#1320,.T.);
#513=FACE_BOUND('',#1321,.T.);
#514=FACE_BOUND('',#1322,.T.);
#515=FACE_BOUND('',#1323,.T.);
#516=FACE_BOUND('',#1355,.T.);
#517=FACE_BOUND('',#1360,.T.);
#518=FACE_BOUND('',#1361,.T.);
#519=FACE_BOUND('',#1362,.T.);
#520=FACE_BOUND('',#1363,.T.);
#521=FACE_BOUND('',#1364,.T.);
#522=FACE_BOUND('',#1365,.T.);
#523=FACE_BOUND('',#1367,.T.);
#524=FACE_BOUND('',#1368,.T.);
#525=FACE_BOUND('',#1369,.T.);
#526=FACE_BOUND('',#1370,.T.);
#527=FACE_BOUND('',#1371,.T.);
#528=FACE_BOUND('',#1373,.T.);
#529=FACE_BOUND('',#1374,.T.);
#530=FACE_BOUND('',#1375,.T.);
#531=FACE_BOUND('',#1376,.T.);
#532=FACE_BOUND('',#1377,.T.);
#533=FACE_BOUND('',#1385,.T.);
#534=FACE_BOUND('',#1386,.T.);
#535=FACE_BOUND('',#1387,.T.);
#536=FACE_BOUND('',#1388,.T.);
#537=FACE_BOUND('',#1389,.T.);
#538=FACE_BOUND('',#1390,.T.);
#539=FACE_BOUND('',#1393,.T.);
#540=FACE_BOUND('',#1398,.T.);
#541=FACE_BOUND('',#1399,.T.);
#542=FACE_BOUND('',#1400,.T.);
#543=FACE_BOUND('',#1401,.T.);
#544=FACE_BOUND('',#1408,.T.);
#545=FACE_BOUND('',#1412,.T.);
#546=FACE_BOUND('',#1413,.T.);
#547=FACE_BOUND('',#1414,.T.);
#548=FACE_BOUND('',#1415,.T.);
#549=FACE_BOUND('',#1416,.T.);
#550=FACE_BOUND('',#1418,.T.);
#551=FACE_BOUND('',#1419,.T.);
#552=FACE_BOUND('',#1420,.T.);
#553=FACE_BOUND('',#1421,.T.);
#554=FACE_BOUND('',#1422,.T.);
#555=FACE_BOUND('',#1429,.T.);
#556=FACE_BOUND('',#1433,.T.);
#557=FACE_BOUND('',#1434,.T.);
#558=FACE_BOUND('',#1435,.T.);
#559=FACE_BOUND('',#1436,.T.);
#560=FACE_BOUND('',#1437,.T.);
#561=FACE_BOUND('',#1439,.T.);
#562=FACE_BOUND('',#1440,.T.);
#563=FACE_BOUND('',#1441,.T.);
#564=FACE_BOUND('',#1442,.T.);
#565=FACE_BOUND('',#1443,.T.);
#566=FACE_BOUND('',#1446,.T.);
#567=FACE_BOUND('',#1449,.T.);
#568=FACE_BOUND('',#1452,.T.);
#569=FACE_BOUND('',#1455,.T.);
#570=FACE_BOUND('',#1462,.T.);
#571=FACE_BOUND('',#1466,.T.);
#572=FACE_BOUND('',#1467,.T.);
#573=FACE_BOUND('',#1468,.T.);
#574=FACE_BOUND('',#1469,.T.);
#575=FACE_BOUND('',#1470,.T.);
#576=FACE_BOUND('',#1472,.T.);
#577=FACE_BOUND('',#1473,.T.);
#578=FACE_BOUND('',#1474,.T.);
#579=FACE_BOUND('',#1475,.T.);
#580=FACE_BOUND('',#1476,.T.);
#581=FACE_BOUND('',#1493,.T.);
#582=FACE_BOUND('',#1494,.T.);
#583=FACE_BOUND('',#1505,.T.);
#584=FACE_BOUND('',#1506,.T.);
#585=FACE_BOUND('',#1510,.T.);
#586=FACE_BOUND('',#1513,.T.);
#587=FACE_BOUND('',#1530,.T.);
#588=FACE_BOUND('',#1538,.T.);
#589=FACE_BOUND('',#1541,.T.);
#590=FACE_BOUND('',#1546,.T.);
#591=FACE_BOUND('',#1551,.T.);
#592=FACE_BOUND('',#1579,.T.);
#593=FACE_BOUND('',#1582,.T.);
#594=FACE_BOUND('',#1585,.T.);
#595=FACE_BOUND('',#1588,.T.);
#596=FACE_BOUND('',#1591,.T.);
#597=FACE_BOUND('',#1599,.T.);
#598=FACE_BOUND('',#1602,.T.);
#599=FACE_BOUND('',#1605,.T.);
#600=FACE_BOUND('',#1608,.T.);
#601=FACE_BOUND('',#1611,.T.);
#602=FACE_BOUND('',#1614,.T.);
#603=FACE_BOUND('',#1616,.T.);
#604=FACE_BOUND('',#1622,.T.);
#605=FACE_BOUND('',#1624,.T.);
#606=FACE_BOUND('',#1626,.T.);
#607=FACE_BOUND('',#1628,.T.);
#608=FACE_BOUND('',#1638,.T.);
#609=FACE_BOUND('',#1646,.T.);
#610=FACE_BOUND('',#1653,.T.);
#611=FACE_BOUND('',#1654,.T.);
#612=FACE_BOUND('',#1661,.T.);
#613=FACE_BOUND('',#1664,.T.);
#614=FACE_BOUND('',#1667,.T.);
#615=FACE_BOUND('',#1676,.T.);
#616=FACE_BOUND('',#1678,.T.);
#617=FACE_BOUND('',#1683,.T.);
#618=FACE_BOUND('',#1685,.T.);
#619=FACE_BOUND('',#1687,.T.);
#620=FACE_BOUND('',#1689,.T.);
#621=FACE_BOUND('',#1695,.T.);
#622=FACE_BOUND('',#1697,.T.);
#623=FACE_BOUND('',#1702,.T.);
#624=FACE_BOUND('',#1704,.T.);
#625=FACE_BOUND('',#1708,.T.);
#626=FACE_BOUND('',#1710,.T.);
#627=FACE_BOUND('',#1714,.T.);
#628=FACE_BOUND('',#1716,.T.);
#629=FACE_BOUND('',#1720,.T.);
#630=FACE_BOUND('',#1722,.T.);
#631=FACE_BOUND('',#1726,.T.);
#632=FACE_BOUND('',#1728,.T.);
#633=FACE_BOUND('',#1738,.T.);
#634=FACE_BOUND('',#1755,.T.);
#635=FACE_BOUND('',#1763,.T.);
#636=FACE_BOUND('',#1781,.T.);
#637=FACE_BOUND('',#1782,.T.);
#638=FACE_BOUND('',#1786,.T.);
#639=FACE_BOUND('',#1787,.T.);
#640=FACE_BOUND('',#1791,.T.);
#641=FACE_BOUND('',#1793,.T.);
#642=FACE_BOUND('',#1797,.T.);
#643=FACE_BOUND('',#1799,.T.);
#644=FACE_BOUND('',#1803,.T.);
#645=FACE_BOUND('',#1819,.T.);
#646=FACE_BOUND('',#1821,.T.);
#647=FACE_BOUND('',#1826,.T.);
#648=FACE_BOUND('',#1828,.T.);
#649=FACE_BOUND('',#1830,.T.);
#650=FACE_BOUND('',#1846,.T.);
#651=PLANE('',#7066);
#652=PLANE('',#7067);
#653=PLANE('',#7068);
#654=PLANE('',#7069);
#655=PLANE('',#7070);
#656=PLANE('',#7071);
#657=PLANE('',#7073);
#658=PLANE('',#7074);
#659=PLANE('',#7075);
#660=PLANE('',#7076);
#661=PLANE('',#7077);
#662=PLANE('',#7078);
#663=PLANE('',#7080);
#664=PLANE('',#7081);
#665=PLANE('',#7082);
#666=PLANE('',#7083);
#667=PLANE('',#7084);
#668=PLANE('',#7085);
#669=PLANE('',#7093);
#670=PLANE('',#7097);
#671=PLANE('',#7101);
#672=PLANE('',#7105);
#673=PLANE('',#7133);
#674=PLANE('',#7143);
#675=PLANE('',#7145);
#676=PLANE('',#7146);
#677=PLANE('',#7147);
#678=PLANE('',#7148);
#679=PLANE('',#7149);
#680=PLANE('',#7150);
#681=PLANE('',#7151);
#682=PLANE('',#7154);
#683=PLANE('',#7155);
#684=PLANE('',#7156);
#685=PLANE('',#7157);
#686=PLANE('',#7158);
#687=PLANE('',#7159);
#688=PLANE('',#7160);
#689=PLANE('',#7177);
#690=PLANE('',#7184);
#691=PLANE('',#7185);
#692=PLANE('',#7202);
#693=PLANE('',#7209);
#694=PLANE('',#7210);
#695=PLANE('',#7215);
#696=PLANE('',#7220);
#697=PLANE('',#7225);
#698=PLANE('',#7230);
#699=PLANE('',#7243);
#700=PLANE('',#7250);
#701=PLANE('',#7251);
#702=PLANE('',#7253);
#703=PLANE('',#7254);
#704=PLANE('',#7255);
#705=PLANE('',#7256);
#706=PLANE('',#7257);
#707=PLANE('',#7258);
#708=PLANE('',#7263);
#709=PLANE('',#7267);
#710=PLANE('',#7268);
#711=PLANE('',#7269);
#712=PLANE('',#7270);
#713=PLANE('',#7271);
#714=PLANE('',#7272);
#715=PLANE('',#7273);
#716=PLANE('',#7278);
#717=PLANE('',#7282);
#718=PLANE('',#7283);
#719=PLANE('',#7284);
#720=PLANE('',#7285);
#721=PLANE('',#7286);
#722=PLANE('',#7287);
#723=PLANE('',#7288);
#724=PLANE('',#7293);
#725=PLANE('',#7294);
#726=PLANE('',#7299);
#727=PLANE('',#7302);
#728=PLANE('',#7304);
#729=PLANE('',#7305);
#730=PLANE('',#7306);
#731=PLANE('',#7307);
#732=PLANE('',#7308);
#733=PLANE('',#7309);
#734=PLANE('',#7310);
#735=PLANE('',#7311);
#736=PLANE('',#7312);
#737=PLANE('',#7314);
#738=PLANE('',#7322);
#739=PLANE('',#7342);
#740=PLANE('',#7345);
#741=PLANE('',#7357);
#742=PLANE('',#7366);
#743=PLANE('',#7399);
#744=PLANE('',#7404);
#745=PLANE('',#7409);
#746=PLANE('',#7414);
#747=PLANE('',#7419);
#748=PLANE('',#7424);
#749=PLANE('',#7433);
#750=PLANE('',#7437);
#751=PLANE('',#7438);
#752=PLANE('',#7440);
#753=PLANE('',#7445);
#754=PLANE('',#7448);
#755=PLANE('',#7453);
#756=PLANE('',#7463);
#757=PLANE('',#7465);
#758=PLANE('',#7466);
#759=PLANE('',#7468);
#760=PLANE('',#7469);
#761=PLANE('',#7470);
#762=PLANE('',#7475);
#763=PLANE('',#7479);
#764=PLANE('',#7483);
#765=PLANE('',#7487);
#766=PLANE('',#7491);
#767=PLANE('',#7495);
#768=PLANE('',#7498);
#769=PLANE('',#7499);
#770=PLANE('',#7502);
#771=PLANE('',#7503);
#772=PLANE('',#7508);
#773=PLANE('',#7514);
#774=PLANE('',#7515);
#775=PLANE('',#7516);
#776=PLANE('',#7517);
#777=PLANE('',#7518);
#778=PLANE('',#7519);
#779=PLANE('',#7520);
#780=PLANE('',#7521);
#781=PLANE('',#7522);
#782=PLANE('',#7527);
#783=PLANE('',#7528);
#784=PLANE('',#7536);
#785=PLANE('',#7551);
#786=PLANE('',#7557);
#787=PLANE('',#7558);
#788=PLANE('',#7560);
#789=PLANE('',#7563);
#790=PLANE('',#7564);
#791=PLANE('',#7566);
#792=PLANE('',#7567);
#793=PLANE('',#7571);
#794=PLANE('',#7579);
#795=PLANE('',#7580);
#796=PLANE('',#7588);
#797=PLANE('',#7589);
#798=PLANE('',#7591);
#799=PLANE('',#7596);
#800=PLANE('',#7603);
#801=PLANE('',#7604);
#802=PLANE('',#7609);
#803=PLANE('',#7613);
#804=PLANE('',#7614);
#805=PLANE('',#7617);
#806=PLANE('',#7625);
#807=PLANE('',#7626);
#808=PLANE('',#7634);
#809=PLANE('',#7635);
#810=PLANE('',#7643);
#811=PLANE('',#7644);
#812=PLANE('',#7652);
#813=PLANE('',#7653);
#814=PLANE('',#7661);
#815=PLANE('',#7662);
#816=PLANE('',#7664);
#817=PLANE('',#7666);
#818=PLANE('',#7667);
#819=PLANE('',#7668);
#820=PLANE('',#7669);
#821=PLANE('',#7670);
#822=PLANE('',#7671);
#823=PLANE('',#7672);
#824=PLANE('',#7673);
#825=PLANE('',#7679);
#826=PLANE('',#7680);
#827=PLANE('',#7681);
#828=PLANE('',#7682);
#829=PLANE('',#7683);
#830=PLANE('',#7684);
#831=PLANE('',#7685);
#832=PLANE('',#7686);
#833=PLANE('',#7687);
#834=PLANE('',#7689);
#835=PLANE('',#7697);
#836=PLANE('',#7703);
#837=PLANE('',#7711);
#838=PLANE('',#7719);
#839=PLANE('',#7720);
#840=PLANE('',#7721);
#841=PLANE('',#7722);
#842=PLANE('',#7723);
#843=PLANE('',#7724);
#844=PLANE('',#7725);
#845=PLANE('',#7726);
#846=PLANE('',#7727);
#847=PLANE('',#7784);
#848=PLANE('',#7785);
#849=PLANE('',#7787);
#850=PLANE('',#7790);
#851=PLANE('',#7798);
#852=PLANE('',#7799);
#853=PLANE('',#7807);
#854=PLANE('',#7808);
#855=PLANE('',#7817);
#856=PLANE('',#7818);
#857=PLANE('',#7819);
#858=PLANE('',#7820);
#859=PLANE('',#7822);
#860=PLANE('',#7823);
#861=PLANE('',#7824);
#862=PLANE('',#7825);
#863=PLANE('',#7830);
#864=PLANE('',#7835);
#865=PLANE('',#7836);
#866=PLANE('',#7837);
#867=PLANE('',#7843);
#868=PLANE('',#7847);
#869=PLANE('',#7848);
#870=PLANE('',#7849);
#871=PLANE('',#7850);
#872=PLANE('',#7851);
#873=PLANE('',#7852);
#874=PLANE('',#7854);
#875=PLANE('',#7859);
#876=PLANE('',#7862);
#877=PLANE('',#7867);
#878=PLANE('',#7868);
#879=PLANE('',#7870);
#880=PLANE('',#7871);
#881=PLANE('',#7872);
#882=PLANE('',#7873);
#883=PLANE('',#7874);
#884=PLANE('',#7875);
#885=PLANE('',#7876);
#886=PLANE('',#7877);
#887=PLANE('',#7885);
#888=FACE_OUTER_BOUND('',#1294,.T.);
#889=FACE_OUTER_BOUND('',#1295,.T.);
#890=FACE_OUTER_BOUND('',#1296,.T.);
#891=FACE_OUTER_BOUND('',#1297,.T.);
#892=FACE_OUTER_BOUND('',#1298,.T.);
#893=FACE_OUTER_BOUND('',#1299,.T.);
#894=FACE_OUTER_BOUND('',#1300,.T.);
#895=FACE_OUTER_BOUND('',#1301,.T.);
#896=FACE_OUTER_BOUND('',#1302,.T.);
#897=FACE_OUTER_BOUND('',#1303,.T.);
#898=FACE_OUTER_BOUND('',#1304,.T.);
#899=FACE_OUTER_BOUND('',#1305,.T.);
#900=FACE_OUTER_BOUND('',#1306,.T.);
#901=FACE_OUTER_BOUND('',#1315,.T.);
#902=FACE_OUTER_BOUND('',#1324,.T.);
#903=FACE_OUTER_BOUND('',#1325,.T.);
#904=FACE_OUTER_BOUND('',#1326,.T.);
#905=FACE_OUTER_BOUND('',#1327,.T.);
#906=FACE_OUTER_BOUND('',#1328,.T.);
#907=FACE_OUTER_BOUND('',#1329,.T.);
#908=FACE_OUTER_BOUND('',#1330,.T.);
#909=FACE_OUTER_BOUND('',#1331,.T.);
#910=FACE_OUTER_BOUND('',#1332,.T.);
#911=FACE_OUTER_BOUND('',#1333,.T.);
#912=FACE_OUTER_BOUND('',#1334,.T.);
#913=FACE_OUTER_BOUND('',#1335,.T.);
#914=FACE_OUTER_BOUND('',#1336,.T.);
#915=FACE_OUTER_BOUND('',#1337,.T.);
#916=FACE_OUTER_BOUND('',#1338,.T.);
#917=FACE_OUTER_BOUND('',#1339,.T.);
#918=FACE_OUTER_BOUND('',#1340,.T.);
#919=FACE_OUTER_BOUND('',#1341,.T.);
#920=FACE_OUTER_BOUND('',#1342,.T.);
#921=FACE_OUTER_BOUND('',#1343,.T.);
#922=FACE_OUTER_BOUND('',#1344,.T.);
#923=FACE_OUTER_BOUND('',#1345,.T.);
#924=FACE_OUTER_BOUND('',#1346,.T.);
#925=FACE_OUTER_BOUND('',#1347,.T.);
#926=FACE_OUTER_BOUND('',#1348,.T.);
#927=FACE_OUTER_BOUND('',#1349,.T.);
#928=FACE_OUTER_BOUND('',#1350,.T.);
#929=FACE_OUTER_BOUND('',#1351,.T.);
#930=FACE_OUTER_BOUND('',#1352,.T.);
#931=FACE_OUTER_BOUND('',#1353,.T.);
#932=FACE_OUTER_BOUND('',#1354,.T.);
#933=FACE_OUTER_BOUND('',#1356,.T.);
#934=FACE_OUTER_BOUND('',#1357,.T.);
#935=FACE_OUTER_BOUND('',#1358,.T.);
#936=FACE_OUTER_BOUND('',#1359,.T.);
#937=FACE_OUTER_BOUND('',#1366,.T.);
#938=FACE_OUTER_BOUND('',#1372,.T.);
#939=FACE_OUTER_BOUND('',#1378,.T.);
#940=FACE_OUTER_BOUND('',#1379,.T.);
#941=FACE_OUTER_BOUND('',#1380,.T.);
#942=FACE_OUTER_BOUND('',#1381,.T.);
#943=FACE_OUTER_BOUND('',#1382,.T.);
#944=FACE_OUTER_BOUND('',#1383,.T.);
#945=FACE_OUTER_BOUND('',#1384,.T.);
#946=FACE_OUTER_BOUND('',#1391,.T.);
#947=FACE_OUTER_BOUND('',#1392,.T.);
#948=FACE_OUTER_BOUND('',#1394,.T.);
#949=FACE_OUTER_BOUND('',#1395,.T.);
#950=FACE_OUTER_BOUND('',#1396,.T.);
#951=FACE_OUTER_BOUND('',#1397,.T.);
#952=FACE_OUTER_BOUND('',#1402,.T.);
#953=FACE_OUTER_BOUND('',#1403,.T.);
#954=FACE_OUTER_BOUND('',#1404,.T.);
#955=FACE_OUTER_BOUND('',#1405,.T.);
#956=FACE_OUTER_BOUND('',#1406,.T.);
#957=FACE_OUTER_BOUND('',#1407,.T.);
#958=FACE_OUTER_BOUND('',#1409,.T.);
#959=FACE_OUTER_BOUND('',#1410,.T.);
#960=FACE_OUTER_BOUND('',#1411,.T.);
#961=FACE_OUTER_BOUND('',#1417,.T.);
#962=FACE_OUTER_BOUND('',#1423,.T.);
#963=FACE_OUTER_BOUND('',#1424,.T.);
#964=FACE_OUTER_BOUND('',#1425,.T.);
#965=FACE_OUTER_BOUND('',#1426,.T.);
#966=FACE_OUTER_BOUND('',#1427,.T.);
#967=FACE_OUTER_BOUND('',#1428,.T.);
#968=FACE_OUTER_BOUND('',#1430,.T.);
#969=FACE_OUTER_BOUND('',#1431,.T.);
#970=FACE_OUTER_BOUND('',#1432,.T.);
#971=FACE_OUTER_BOUND('',#1438,.T.);
#972=FACE_OUTER_BOUND('',#1444,.T.);
#973=FACE_OUTER_BOUND('',#1445,.T.);
#974=FACE_OUTER_BOUND('',#1447,.T.);
#975=FACE_OUTER_BOUND('',#1448,.T.);
#976=FACE_OUTER_BOUND('',#1450,.T.);
#977=FACE_OUTER_BOUND('',#1451,.T.);
#978=FACE_OUTER_BOUND('',#1453,.T.);
#979=FACE_OUTER_BOUND('',#1454,.T.);
#980=FACE_OUTER_BOUND('',#1456,.T.);
#981=FACE_OUTER_BOUND('',#1457,.T.);
#982=FACE_OUTER_BOUND('',#1458,.T.);
#983=FACE_OUTER_BOUND('',#1459,.T.);
#984=FACE_OUTER_BOUND('',#1460,.T.);
#985=FACE_OUTER_BOUND('',#1461,.T.);
#986=FACE_OUTER_BOUND('',#1463,.T.);
#987=FACE_OUTER_BOUND('',#1464,.T.);
#988=FACE_OUTER_BOUND('',#1465,.T.);
#989=FACE_OUTER_BOUND('',#1471,.T.);
#990=FACE_OUTER_BOUND('',#1477,.T.);
#991=FACE_OUTER_BOUND('',#1478,.T.);
#992=FACE_OUTER_BOUND('',#1479,.T.);
#993=FACE_OUTER_BOUND('',#1480,.T.);
#994=FACE_OUTER_BOUND('',#1481,.T.);
#995=FACE_OUTER_BOUND('',#1482,.T.);
#996=FACE_OUTER_BOUND('',#1483,.T.);
#997=FACE_OUTER_BOUND('',#1484,.T.);
#998=FACE_OUTER_BOUND('',#1485,.T.);
#999=FACE_OUTER_BOUND('',#1486,.T.);
#1000=FACE_OUTER_BOUND('',#1487,.T.);
#1001=FACE_OUTER_BOUND('',#1488,.T.);
#1002=FACE_OUTER_BOUND('',#1489,.T.);
#1003=FACE_OUTER_BOUND('',#1490,.T.);
#1004=FACE_OUTER_BOUND('',#1491,.T.);
#1005=FACE_OUTER_BOUND('',#1492,.T.);
#1006=FACE_OUTER_BOUND('',#1495,.T.);
#1007=FACE_OUTER_BOUND('',#1496,.T.);
#1008=FACE_OUTER_BOUND('',#1497,.T.);
#1009=FACE_OUTER_BOUND('',#1498,.T.);
#1010=FACE_OUTER_BOUND('',#1499,.T.);
#1011=FACE_OUTER_BOUND('',#1500,.T.);
#1012=FACE_OUTER_BOUND('',#1501,.T.);
#1013=FACE_OUTER_BOUND('',#1502,.T.);
#1014=FACE_OUTER_BOUND('',#1503,.T.);
#1015=FACE_OUTER_BOUND('',#1504,.T.);
#1016=FACE_OUTER_BOUND('',#1507,.T.);
#1017=FACE_OUTER_BOUND('',#1508,.T.);
#1018=FACE_OUTER_BOUND('',#1509,.T.);
#1019=FACE_OUTER_BOUND('',#1511,.T.);
#1020=FACE_OUTER_BOUND('',#1512,.T.);
#1021=FACE_OUTER_BOUND('',#1514,.T.);
#1022=FACE_OUTER_BOUND('',#1515,.T.);
#1023=FACE_OUTER_BOUND('',#1516,.T.);
#1024=FACE_OUTER_BOUND('',#1517,.T.);
#1025=FACE_OUTER_BOUND('',#1518,.T.);
#1026=FACE_OUTER_BOUND('',#1519,.T.);
#1027=FACE_OUTER_BOUND('',#1520,.T.);
#1028=FACE_OUTER_BOUND('',#1521,.T.);
#1029=FACE_OUTER_BOUND('',#1522,.T.);
#1030=FACE_OUTER_BOUND('',#1523,.T.);
#1031=FACE_OUTER_BOUND('',#1524,.T.);
#1032=FACE_OUTER_BOUND('',#1525,.T.);
#1033=FACE_OUTER_BOUND('',#1526,.T.);
#1034=FACE_OUTER_BOUND('',#1527,.T.);
#1035=FACE_OUTER_BOUND('',#1528,.T.);
#1036=FACE_OUTER_BOUND('',#1529,.T.);
#1037=FACE_OUTER_BOUND('',#1531,.T.);
#1038=FACE_OUTER_BOUND('',#1532,.T.);
#1039=FACE_OUTER_BOUND('',#1533,.T.);
#1040=FACE_OUTER_BOUND('',#1534,.T.);
#1041=FACE_OUTER_BOUND('',#1535,.T.);
#1042=FACE_OUTER_BOUND('',#1536,.T.);
#1043=FACE_OUTER_BOUND('',#1537,.T.);
#1044=FACE_OUTER_BOUND('',#1539,.T.);
#1045=FACE_OUTER_BOUND('',#1540,.T.);
#1046=FACE_OUTER_BOUND('',#1542,.T.);
#1047=FACE_OUTER_BOUND('',#1543,.T.);
#1048=FACE_OUTER_BOUND('',#1544,.T.);
#1049=FACE_OUTER_BOUND('',#1545,.T.);
#1050=FACE_OUTER_BOUND('',#1547,.T.);
#1051=FACE_OUTER_BOUND('',#1548,.T.);
#1052=FACE_OUTER_BOUND('',#1549,.T.);
#1053=FACE_OUTER_BOUND('',#1550,.T.);
#1054=FACE_OUTER_BOUND('',#1552,.T.);
#1055=FACE_OUTER_BOUND('',#1553,.T.);
#1056=FACE_OUTER_BOUND('',#1554,.T.);
#1057=FACE_OUTER_BOUND('',#1555,.T.);
#1058=FACE_OUTER_BOUND('',#1556,.T.);
#1059=FACE_OUTER_BOUND('',#1557,.T.);
#1060=FACE_OUTER_BOUND('',#1558,.T.);
#1061=FACE_OUTER_BOUND('',#1559,.T.);
#1062=FACE_OUTER_BOUND('',#1560,.T.);
#1063=FACE_OUTER_BOUND('',#1561,.T.);
#1064=FACE_OUTER_BOUND('',#1562,.T.);
#1065=FACE_OUTER_BOUND('',#1563,.T.);
#1066=FACE_OUTER_BOUND('',#1564,.T.);
#1067=FACE_OUTER_BOUND('',#1565,.T.);
#1068=FACE_OUTER_BOUND('',#1566,.T.);
#1069=FACE_OUTER_BOUND('',#1567,.T.);
#1070=FACE_OUTER_BOUND('',#1568,.T.);
#1071=FACE_OUTER_BOUND('',#1569,.T.);
#1072=FACE_OUTER_BOUND('',#1570,.T.);
#1073=FACE_OUTER_BOUND('',#1571,.T.);
#1074=FACE_OUTER_BOUND('',#1572,.T.);
#1075=FACE_OUTER_BOUND('',#1573,.T.);
#1076=FACE_OUTER_BOUND('',#1574,.T.);
#1077=FACE_OUTER_BOUND('',#1575,.T.);
#1078=FACE_OUTER_BOUND('',#1576,.T.);
#1079=FACE_OUTER_BOUND('',#1577,.T.);
#1080=FACE_OUTER_BOUND('',#1578,.T.);
#1081=FACE_OUTER_BOUND('',#1580,.T.);
#1082=FACE_OUTER_BOUND('',#1581,.T.);
#1083=FACE_OUTER_BOUND('',#1583,.T.);
#1084=FACE_OUTER_BOUND('',#1584,.T.);
#1085=FACE_OUTER_BOUND('',#1586,.T.);
#1086=FACE_OUTER_BOUND('',#1587,.T.);
#1087=FACE_OUTER_BOUND('',#1589,.T.);
#1088=FACE_OUTER_BOUND('',#1590,.T.);
#1089=FACE_OUTER_BOUND('',#1592,.T.);
#1090=FACE_OUTER_BOUND('',#1593,.T.);
#1091=FACE_OUTER_BOUND('',#1594,.T.);
#1092=FACE_OUTER_BOUND('',#1595,.T.);
#1093=FACE_OUTER_BOUND('',#1596,.T.);
#1094=FACE_OUTER_BOUND('',#1597,.T.);
#1095=FACE_OUTER_BOUND('',#1598,.T.);
#1096=FACE_OUTER_BOUND('',#1600,.T.);
#1097=FACE_OUTER_BOUND('',#1601,.T.);
#1098=FACE_OUTER_BOUND('',#1603,.T.);
#1099=FACE_OUTER_BOUND('',#1604,.T.);
#1100=FACE_OUTER_BOUND('',#1606,.T.);
#1101=FACE_OUTER_BOUND('',#1607,.T.);
#1102=FACE_OUTER_BOUND('',#1609,.T.);
#1103=FACE_OUTER_BOUND('',#1610,.T.);
#1104=FACE_OUTER_BOUND('',#1612,.T.);
#1105=FACE_OUTER_BOUND('',#1613,.T.);
#1106=FACE_OUTER_BOUND('',#1615,.T.);
#1107=FACE_OUTER_BOUND('',#1617,.T.);
#1108=FACE_OUTER_BOUND('',#1618,.T.);
#1109=FACE_OUTER_BOUND('',#1619,.T.);
#1110=FACE_OUTER_BOUND('',#1620,.T.);
#1111=FACE_OUTER_BOUND('',#1621,.T.);
#1112=FACE_OUTER_BOUND('',#1623,.T.);
#1113=FACE_OUTER_BOUND('',#1625,.T.);
#1114=FACE_OUTER_BOUND('',#1627,.T.);
#1115=FACE_OUTER_BOUND('',#1629,.T.);
#1116=FACE_OUTER_BOUND('',#1630,.T.);
#1117=FACE_OUTER_BOUND('',#1631,.T.);
#1118=FACE_OUTER_BOUND('',#1632,.T.);
#1119=FACE_OUTER_BOUND('',#1633,.T.);
#1120=FACE_OUTER_BOUND('',#1634,.T.);
#1121=FACE_OUTER_BOUND('',#1635,.T.);
#1122=FACE_OUTER_BOUND('',#1636,.T.);
#1123=FACE_OUTER_BOUND('',#1637,.T.);
#1124=FACE_OUTER_BOUND('',#1639,.T.);
#1125=FACE_OUTER_BOUND('',#1640,.T.);
#1126=FACE_OUTER_BOUND('',#1641,.T.);
#1127=FACE_OUTER_BOUND('',#1642,.T.);
#1128=FACE_OUTER_BOUND('',#1643,.T.);
#1129=FACE_OUTER_BOUND('',#1644,.T.);
#1130=FACE_OUTER_BOUND('',#1645,.T.);
#1131=FACE_OUTER_BOUND('',#1647,.T.);
#1132=FACE_OUTER_BOUND('',#1648,.T.);
#1133=FACE_OUTER_BOUND('',#1649,.T.);
#1134=FACE_OUTER_BOUND('',#1650,.T.);
#1135=FACE_OUTER_BOUND('',#1651,.T.);
#1136=FACE_OUTER_BOUND('',#1652,.T.);
#1137=FACE_OUTER_BOUND('',#1655,.T.);
#1138=FACE_OUTER_BOUND('',#1656,.T.);
#1139=FACE_OUTER_BOUND('',#1657,.T.);
#1140=FACE_OUTER_BOUND('',#1658,.T.);
#1141=FACE_OUTER_BOUND('',#1659,.T.);
#1142=FACE_OUTER_BOUND('',#1660,.T.);
#1143=FACE_OUTER_BOUND('',#1662,.T.);
#1144=FACE_OUTER_BOUND('',#1663,.T.);
#1145=FACE_OUTER_BOUND('',#1665,.T.);
#1146=FACE_OUTER_BOUND('',#1666,.T.);
#1147=FACE_OUTER_BOUND('',#1668,.T.);
#1148=FACE_OUTER_BOUND('',#1669,.T.);
#1149=FACE_OUTER_BOUND('',#1670,.T.);
#1150=FACE_OUTER_BOUND('',#1671,.T.);
#1151=FACE_OUTER_BOUND('',#1672,.T.);
#1152=FACE_OUTER_BOUND('',#1673,.T.);
#1153=FACE_OUTER_BOUND('',#1674,.T.);
#1154=FACE_OUTER_BOUND('',#1675,.T.);
#1155=FACE_OUTER_BOUND('',#1677,.T.);
#1156=FACE_OUTER_BOUND('',#1679,.T.);
#1157=FACE_OUTER_BOUND('',#1680,.T.);
#1158=FACE_OUTER_BOUND('',#1681,.T.);
#1159=FACE_OUTER_BOUND('',#1682,.T.);
#1160=FACE_OUTER_BOUND('',#1684,.T.);
#1161=FACE_OUTER_BOUND('',#1686,.T.);
#1162=FACE_OUTER_BOUND('',#1688,.T.);
#1163=FACE_OUTER_BOUND('',#1690,.T.);
#1164=FACE_OUTER_BOUND('',#1691,.T.);
#1165=FACE_OUTER_BOUND('',#1692,.T.);
#1166=FACE_OUTER_BOUND('',#1693,.T.);
#1167=FACE_OUTER_BOUND('',#1694,.T.);
#1168=FACE_OUTER_BOUND('',#1696,.T.);
#1169=FACE_OUTER_BOUND('',#1698,.T.);
#1170=FACE_OUTER_BOUND('',#1699,.T.);
#1171=FACE_OUTER_BOUND('',#1700,.T.);
#1172=FACE_OUTER_BOUND('',#1701,.T.);
#1173=FACE_OUTER_BOUND('',#1703,.T.);
#1174=FACE_OUTER_BOUND('',#1705,.T.);
#1175=FACE_OUTER_BOUND('',#1706,.T.);
#1176=FACE_OUTER_BOUND('',#1707,.T.);
#1177=FACE_OUTER_BOUND('',#1709,.T.);
#1178=FACE_OUTER_BOUND('',#1711,.T.);
#1179=FACE_OUTER_BOUND('',#1712,.T.);
#1180=FACE_OUTER_BOUND('',#1713,.T.);
#1181=FACE_OUTER_BOUND('',#1715,.T.);
#1182=FACE_OUTER_BOUND('',#1717,.T.);
#1183=FACE_OUTER_BOUND('',#1718,.T.);
#1184=FACE_OUTER_BOUND('',#1719,.T.);
#1185=FACE_OUTER_BOUND('',#1721,.T.);
#1186=FACE_OUTER_BOUND('',#1723,.T.);
#1187=FACE_OUTER_BOUND('',#1724,.T.);
#1188=FACE_OUTER_BOUND('',#1725,.T.);
#1189=FACE_OUTER_BOUND('',#1727,.T.);
#1190=FACE_OUTER_BOUND('',#1729,.T.);
#1191=FACE_OUTER_BOUND('',#1730,.T.);
#1192=FACE_OUTER_BOUND('',#1731,.T.);
#1193=FACE_OUTER_BOUND('',#1732,.T.);
#1194=FACE_OUTER_BOUND('',#1733,.T.);
#1195=FACE_OUTER_BOUND('',#1734,.T.);
#1196=FACE_OUTER_BOUND('',#1735,.T.);
#1197=FACE_OUTER_BOUND('',#1736,.T.);
#1198=FACE_OUTER_BOUND('',#1737,.T.);
#1199=FACE_OUTER_BOUND('',#1739,.T.);
#1200=FACE_OUTER_BOUND('',#1740,.T.);
#1201=FACE_OUTER_BOUND('',#1741,.T.);
#1202=FACE_OUTER_BOUND('',#1742,.T.);
#1203=FACE_OUTER_BOUND('',#1743,.T.);
#1204=FACE_OUTER_BOUND('',#1744,.T.);
#1205=FACE_OUTER_BOUND('',#1745,.T.);
#1206=FACE_OUTER_BOUND('',#1746,.T.);
#1207=FACE_OUTER_BOUND('',#1747,.T.);
#1208=FACE_OUTER_BOUND('',#1748,.T.);
#1209=FACE_OUTER_BOUND('',#1749,.T.);
#1210=FACE_OUTER_BOUND('',#1750,.T.);
#1211=FACE_OUTER_BOUND('',#1751,.T.);
#1212=FACE_OUTER_BOUND('',#1752,.T.);
#1213=FACE_OUTER_BOUND('',#1753,.T.);
#1214=FACE_OUTER_BOUND('',#1754,.T.);
#1215=FACE_OUTER_BOUND('',#1756,.T.);
#1216=FACE_OUTER_BOUND('',#1757,.T.);
#1217=FACE_OUTER_BOUND('',#1758,.T.);
#1218=FACE_OUTER_BOUND('',#1759,.T.);
#1219=FACE_OUTER_BOUND('',#1760,.T.);
#1220=FACE_OUTER_BOUND('',#1761,.T.);
#1221=FACE_OUTER_BOUND('',#1762,.T.);
#1222=FACE_OUTER_BOUND('',#1764,.T.);
#1223=FACE_OUTER_BOUND('',#1765,.T.);
#1224=FACE_OUTER_BOUND('',#1766,.T.);
#1225=FACE_OUTER_BOUND('',#1767,.T.);
#1226=FACE_OUTER_BOUND('',#1768,.T.);
#1227=FACE_OUTER_BOUND('',#1769,.T.);
#1228=FACE_OUTER_BOUND('',#1770,.T.);
#1229=FACE_OUTER_BOUND('',#1771,.T.);
#1230=FACE_OUTER_BOUND('',#1772,.T.);
#1231=FACE_OUTER_BOUND('',#1773,.T.);
#1232=FACE_OUTER_BOUND('',#1774,.T.);
#1233=FACE_OUTER_BOUND('',#1775,.T.);
#1234=FACE_OUTER_BOUND('',#1776,.T.);
#1235=FACE_OUTER_BOUND('',#1777,.T.);
#1236=FACE_OUTER_BOUND('',#1778,.T.);
#1237=FACE_OUTER_BOUND('',#1779,.T.);
#1238=FACE_OUTER_BOUND('',#1780,.T.);
#1239=FACE_OUTER_BOUND('',#1783,.T.);
#1240=FACE_OUTER_BOUND('',#1784,.T.);
#1241=FACE_OUTER_BOUND('',#1785,.T.);
#1242=FACE_OUTER_BOUND('',#1788,.T.);
#1243=FACE_OUTER_BOUND('',#1789,.T.);
#1244=FACE_OUTER_BOUND('',#1790,.T.);
#1245=FACE_OUTER_BOUND('',#1792,.T.);
#1246=FACE_OUTER_BOUND('',#1794,.T.);
#1247=FACE_OUTER_BOUND('',#1795,.T.);
#1248=FACE_OUTER_BOUND('',#1796,.T.);
#1249=FACE_OUTER_BOUND('',#1798,.T.);
#1250=FACE_OUTER_BOUND('',#1800,.T.);
#1251=FACE_OUTER_BOUND('',#1801,.T.);
#1252=FACE_OUTER_BOUND('',#1802,.T.);
#1253=FACE_OUTER_BOUND('',#1804,.T.);
#1254=FACE_OUTER_BOUND('',#1805,.T.);
#1255=FACE_OUTER_BOUND('',#1806,.T.);
#1256=FACE_OUTER_BOUND('',#1807,.T.);
#1257=FACE_OUTER_BOUND('',#1808,.T.);
#1258=FACE_OUTER_BOUND('',#1809,.T.);
#1259=FACE_OUTER_BOUND('',#1810,.T.);
#1260=FACE_OUTER_BOUND('',#1811,.T.);
#1261=FACE_OUTER_BOUND('',#1812,.T.);
#1262=FACE_OUTER_BOUND('',#1813,.T.);
#1263=FACE_OUTER_BOUND('',#1814,.T.);
#1264=FACE_OUTER_BOUND('',#1815,.T.);
#1265=FACE_OUTER_BOUND('',#1816,.T.);
#1266=FACE_OUTER_BOUND('',#1817,.T.);
#1267=FACE_OUTER_BOUND('',#1818,.T.);
#1268=FACE_OUTER_BOUND('',#1820,.T.);
#1269=FACE_OUTER_BOUND('',#1822,.T.);
#1270=FACE_OUTER_BOUND('',#1823,.T.);
#1271=FACE_OUTER_BOUND('',#1824,.T.);
#1272=FACE_OUTER_BOUND('',#1825,.T.);
#1273=FACE_OUTER_BOUND('',#1827,.T.);
#1274=FACE_OUTER_BOUND('',#1829,.T.);
#1275=FACE_OUTER_BOUND('',#1831,.T.);
#1276=FACE_OUTER_BOUND('',#1832,.T.);
#1277=FACE_OUTER_BOUND('',#1833,.T.);
#1278=FACE_OUTER_BOUND('',#1834,.T.);
#1279=FACE_OUTER_BOUND('',#1835,.T.);
#1280=FACE_OUTER_BOUND('',#1836,.T.);
#1281=FACE_OUTER_BOUND('',#1837,.T.);
#1282=FACE_OUTER_BOUND('',#1838,.T.);
#1283=FACE_OUTER_BOUND('',#1839,.T.);
#1284=FACE_OUTER_BOUND('',#1840,.T.);
#1285=FACE_OUTER_BOUND('',#1841,.T.);
#1286=FACE_OUTER_BOUND('',#1842,.T.);
#1287=FACE_OUTER_BOUND('',#1843,.T.);
#1288=FACE_OUTER_BOUND('',#1844,.T.);
#1289=FACE_OUTER_BOUND('',#1845,.T.);
#1290=FACE_OUTER_BOUND('',#1847,.T.);
#1291=FACE_OUTER_BOUND('',#1848,.T.);
#1292=FACE_OUTER_BOUND('',#1849,.T.);
#1293=FACE_OUTER_BOUND('',#1850,.T.);
#1294=EDGE_LOOP('',(#4421,#4422,#4423,#4424));
#1295=EDGE_LOOP('',(#4425,#4426,#4427,#4428));
#1296=EDGE_LOOP('',(#4429,#4430,#4431,#4432));
#1297=EDGE_LOOP('',(#4433,#4434,#4435,#4436));
#1298=EDGE_LOOP('',(#4437,#4438,#4439,#4440));
#1299=EDGE_LOOP('',(#4441,#4442,#4443,#4444));
#1300=EDGE_LOOP('',(#4445,#4446,#4447,#4448));
#1301=EDGE_LOOP('',(#4449,#4450,#4451,#4452));
#1302=EDGE_LOOP('',(#4453,#4454,#4455,#4456));
#1303=EDGE_LOOP('',(#4457,#4458,#4459,#4460));
#1304=EDGE_LOOP('',(#4461,#4462,#4463,#4464));
#1305=EDGE_LOOP('',(#4465,#4466,#4467,#4468));
#1306=EDGE_LOOP('',(#4469,#4470,#4471,#4472));
#1307=EDGE_LOOP('',(#4473));
#1308=EDGE_LOOP('',(#4474));
#1309=EDGE_LOOP('',(#4475));
#1310=EDGE_LOOP('',(#4476));
#1311=EDGE_LOOP('',(#4477));
#1312=EDGE_LOOP('',(#4478));
#1313=EDGE_LOOP('',(#4479));
#1314=EDGE_LOOP('',(#4480));
#1315=EDGE_LOOP('',(#4481,#4482,#4483,#4484));
#1316=EDGE_LOOP('',(#4485));
#1317=EDGE_LOOP('',(#4486));
#1318=EDGE_LOOP('',(#4487));
#1319=EDGE_LOOP('',(#4488));
#1320=EDGE_LOOP('',(#4489));
#1321=EDGE_LOOP('',(#4490));
#1322=EDGE_LOOP('',(#4491));
#1323=EDGE_LOOP('',(#4492));
#1324=EDGE_LOOP('',(#4493,#4494,#4495,#4496));
#1325=EDGE_LOOP('',(#4497,#4498,#4499,#4500));
#1326=EDGE_LOOP('',(#4501,#4502,#4503,#4504));
#1327=EDGE_LOOP('',(#4505,#4506,#4507,#4508));
#1328=EDGE_LOOP('',(#4509,#4510,#4511,#4512));
#1329=EDGE_LOOP('',(#4513,#4514,#4515,#4516));
#1330=EDGE_LOOP('',(#4517,#4518,#4519,#4520));
#1331=EDGE_LOOP('',(#4521,#4522,#4523,#4524));
#1332=EDGE_LOOP('',(#4525,#4526,#4527,#4528));
#1333=EDGE_LOOP('',(#4529,#4530,#4531,#4532));
#1334=EDGE_LOOP('',(#4533,#4534,#4535,#4536));
#1335=EDGE_LOOP('',(#4537,#4538,#4539,#4540));
#1336=EDGE_LOOP('',(#4541,#4542,#4543,#4544));
#1337=EDGE_LOOP('',(#4545,#4546,#4547,#4548));
#1338=EDGE_LOOP('',(#4549));
#1339=EDGE_LOOP('',(#4550,#4551,#4552,#4553));
#1340=EDGE_LOOP('',(#4554));
#1341=EDGE_LOOP('',(#4555,#4556,#4557,#4558));
#1342=EDGE_LOOP('',(#4559));
#1343=EDGE_LOOP('',(#4560,#4561,#4562,#4563));
#1344=EDGE_LOOP('',(#4564));
#1345=EDGE_LOOP('',(#4565,#4566,#4567,#4568));
#1346=EDGE_LOOP('',(#4569,#4570,#4571,#4572));
#1347=EDGE_LOOP('',(#4573,#4574,#4575,#4576));
#1348=EDGE_LOOP('',(#4577,#4578,#4579,#4580));
#1349=EDGE_LOOP('',(#4581,#4582,#4583,#4584));
#1350=EDGE_LOOP('',(#4585,#4586,#4587,#4588));
#1351=EDGE_LOOP('',(#4589,#4590,#4591,#4592));
#1352=EDGE_LOOP('',(#4593,#4594,#4595,#4596));
#1353=EDGE_LOOP('',(#4597,#4598,#4599,#4600));
#1354=EDGE_LOOP('',(#4601));
#1355=EDGE_LOOP('',(#4602));
#1356=EDGE_LOOP('',(#4603,#4604,#4605,#4606));
#1357=EDGE_LOOP('',(#4607,#4608,#4609,#4610));
#1358=EDGE_LOOP('',(#4611,#4612,#4613,#4614));
#1359=EDGE_LOOP('',(#4615,#4616,#4617,#4618,#4619,#4620,#4621,#4622,#4623,
#4624));
#1360=EDGE_LOOP('',(#4625));
#1361=EDGE_LOOP('',(#4626));
#1362=EDGE_LOOP('',(#4627));
#1363=EDGE_LOOP('',(#4628));
#1364=EDGE_LOOP('',(#4629));
#1365=EDGE_LOOP('',(#4630));
#1366=EDGE_LOOP('',(#4631,#4632,#4633,#4634));
#1367=EDGE_LOOP('',(#4635));
#1368=EDGE_LOOP('',(#4636));
#1369=EDGE_LOOP('',(#4637));
#1370=EDGE_LOOP('',(#4638));
#1371=EDGE_LOOP('',(#4639));
#1372=EDGE_LOOP('',(#4640,#4641,#4642,#4643));
#1373=EDGE_LOOP('',(#4644,#4645,#4646,#4647));
#1374=EDGE_LOOP('',(#4648));
#1375=EDGE_LOOP('',(#4649));
#1376=EDGE_LOOP('',(#4650));
#1377=EDGE_LOOP('',(#4651));
#1378=EDGE_LOOP('',(#4652,#4653,#4654,#4655));
#1379=EDGE_LOOP('',(#4656,#4657,#4658,#4659));
#1380=EDGE_LOOP('',(#4660,#4661,#4662,#4663));
#1381=EDGE_LOOP('',(#4664,#4665,#4666,#4667));
#1382=EDGE_LOOP('',(#4668,#4669,#4670,#4671));
#1383=EDGE_LOOP('',(#4672,#4673,#4674,#4675));
#1384=EDGE_LOOP('',(#4676,#4677,#4678,#4679,#4680,#4681,#4682,#4683,#4684,
#4685));
#1385=EDGE_LOOP('',(#4686));
#1386=EDGE_LOOP('',(#4687));
#1387=EDGE_LOOP('',(#4688));
#1388=EDGE_LOOP('',(#4689));
#1389=EDGE_LOOP('',(#4690));
#1390=EDGE_LOOP('',(#4691));
#1391=EDGE_LOOP('',(#4692,#4693,#4694,#4695));
#1392=EDGE_LOOP('',(#4696,#4697,#4698,#4699));
#1393=EDGE_LOOP('',(#4700));
#1394=EDGE_LOOP('',(#4701,#4702,#4703,#4704));
#1395=EDGE_LOOP('',(#4705,#4706,#4707,#4708));
#1396=EDGE_LOOP('',(#4709,#4710,#4711,#4712));
#1397=EDGE_LOOP('',(#4713,#4714,#4715,#4716));
#1398=EDGE_LOOP('',(#4717));
#1399=EDGE_LOOP('',(#4718));
#1400=EDGE_LOOP('',(#4719));
#1401=EDGE_LOOP('',(#4720));
#1402=EDGE_LOOP('',(#4721,#4722,#4723,#4724));
#1403=EDGE_LOOP('',(#4725,#4726,#4727,#4728));
#1404=EDGE_LOOP('',(#4729,#4730,#4731,#4732));
#1405=EDGE_LOOP('',(#4733,#4734,#4735,#4736));
#1406=EDGE_LOOP('',(#4737,#4738,#4739,#4740));
#1407=EDGE_LOOP('',(#4741));
#1408=EDGE_LOOP('',(#4742));
#1409=EDGE_LOOP('',(#4743,#4744,#4745,#4746));
#1410=EDGE_LOOP('',(#4747,#4748,#4749,#4750));
#1411=EDGE_LOOP('',(#4751));
#1412=EDGE_LOOP('',(#4752));
#1413=EDGE_LOOP('',(#4753));
#1414=EDGE_LOOP('',(#4754));
#1415=EDGE_LOOP('',(#4755));
#1416=EDGE_LOOP('',(#4756));
#1417=EDGE_LOOP('',(#4757));
#1418=EDGE_LOOP('',(#4758));
#1419=EDGE_LOOP('',(#4759));
#1420=EDGE_LOOP('',(#4760));
#1421=EDGE_LOOP('',(#4761));
#1422=EDGE_LOOP('',(#4762));
#1423=EDGE_LOOP('',(#4763,#4764,#4765,#4766));
#1424=EDGE_LOOP('',(#4767,#4768,#4769,#4770));
#1425=EDGE_LOOP('',(#4771,#4772,#4773,#4774));
#1426=EDGE_LOOP('',(#4775,#4776,#4777,#4778));
#1427=EDGE_LOOP('',(#4779,#4780,#4781,#4782));
#1428=EDGE_LOOP('',(#4783));
#1429=EDGE_LOOP('',(#4784));
#1430=EDGE_LOOP('',(#4785,#4786,#4787,#4788));
#1431=EDGE_LOOP('',(#4789,#4790,#4791,#4792));
#1432=EDGE_LOOP('',(#4793));
#1433=EDGE_LOOP('',(#4794));
#1434=EDGE_LOOP('',(#4795));
#1435=EDGE_LOOP('',(#4796));
#1436=EDGE_LOOP('',(#4797));
#1437=EDGE_LOOP('',(#4798));
#1438=EDGE_LOOP('',(#4799));
#1439=EDGE_LOOP('',(#4800));
#1440=EDGE_LOOP('',(#4801));
#1441=EDGE_LOOP('',(#4802));
#1442=EDGE_LOOP('',(#4803));
#1443=EDGE_LOOP('',(#4804));
#1444=EDGE_LOOP('',(#4805,#4806,#4807,#4808));
#1445=EDGE_LOOP('',(#4809));
#1446=EDGE_LOOP('',(#4810));
#1447=EDGE_LOOP('',(#4811,#4812,#4813,#4814));
#1448=EDGE_LOOP('',(#4815));
#1449=EDGE_LOOP('',(#4816));
#1450=EDGE_LOOP('',(#4817,#4818,#4819,#4820));
#1451=EDGE_LOOP('',(#4821));
#1452=EDGE_LOOP('',(#4822));
#1453=EDGE_LOOP('',(#4823,#4824,#4825,#4826));
#1454=EDGE_LOOP('',(#4827));
#1455=EDGE_LOOP('',(#4828));
#1456=EDGE_LOOP('',(#4829,#4830,#4831,#4832));
#1457=EDGE_LOOP('',(#4833,#4834,#4835,#4836));
#1458=EDGE_LOOP('',(#4837,#4838,#4839,#4840));
#1459=EDGE_LOOP('',(#4841,#4842,#4843,#4844));
#1460=EDGE_LOOP('',(#4845,#4846,#4847,#4848));
#1461=EDGE_LOOP('',(#4849));
#1462=EDGE_LOOP('',(#4850));
#1463=EDGE_LOOP('',(#4851,#4852,#4853,#4854));
#1464=EDGE_LOOP('',(#4855,#4856,#4857,#4858));
#1465=EDGE_LOOP('',(#4859));
#1466=EDGE_LOOP('',(#4860));
#1467=EDGE_LOOP('',(#4861));
#1468=EDGE_LOOP('',(#4862));
#1469=EDGE_LOOP('',(#4863));
#1470=EDGE_LOOP('',(#4864));
#1471=EDGE_LOOP('',(#4865));
#1472=EDGE_LOOP('',(#4866));
#1473=EDGE_LOOP('',(#4867));
#1474=EDGE_LOOP('',(#4868));
#1475=EDGE_LOOP('',(#4869));
#1476=EDGE_LOOP('',(#4870));
#1477=EDGE_LOOP('',(#4871,#4872,#4873,#4874));
#1478=EDGE_LOOP('',(#4875,#4876,#4877,#4878));
#1479=EDGE_LOOP('',(#4879,#4880,#4881,#4882));
#1480=EDGE_LOOP('',(#4883,#4884,#4885,#4886));
#1481=EDGE_LOOP('',(#4887,#4888,#4889,#4890));
#1482=EDGE_LOOP('',(#4891,#4892,#4893,#4894));
#1483=EDGE_LOOP('',(#4895,#4896,#4897,#4898));
#1484=EDGE_LOOP('',(#4899));
#1485=EDGE_LOOP('',(#4900,#4901,#4902,#4903));
#1486=EDGE_LOOP('',(#4904));
#1487=EDGE_LOOP('',(#4905,#4906,#4907,#4908));
#1488=EDGE_LOOP('',(#4909,#4910,#4911,#4912));
#1489=EDGE_LOOP('',(#4913,#4914,#4915,#4916));
#1490=EDGE_LOOP('',(#4917,#4918,#4919,#4920));
#1491=EDGE_LOOP('',(#4921,#4922,#4923,#4924));
#1492=EDGE_LOOP('',(#4925,#4926,#4927,#4928));
#1493=EDGE_LOOP('',(#4929));
#1494=EDGE_LOOP('',(#4930));
#1495=EDGE_LOOP('',(#4931,#4932,#4933,#4934));
#1496=EDGE_LOOP('',(#4935));
#1497=EDGE_LOOP('',(#4936,#4937,#4938,#4939));
#1498=EDGE_LOOP('',(#4940));
#1499=EDGE_LOOP('',(#4941,#4942,#4943,#4944));
#1500=EDGE_LOOP('',(#4945,#4946,#4947,#4948));
#1501=EDGE_LOOP('',(#4949,#4950,#4951,#4952));
#1502=EDGE_LOOP('',(#4953,#4954,#4955,#4956));
#1503=EDGE_LOOP('',(#4957,#4958,#4959,#4960));
#1504=EDGE_LOOP('',(#4961,#4962,#4963,#4964));
#1505=EDGE_LOOP('',(#4965));
#1506=EDGE_LOOP('',(#4966));
#1507=EDGE_LOOP('',(#4967,#4968,#4969,#4970));
#1508=EDGE_LOOP('',(#4971));
#1509=EDGE_LOOP('',(#4972));
#1510=EDGE_LOOP('',(#4973));
#1511=EDGE_LOOP('',(#4974,#4975,#4976,#4977));
#1512=EDGE_LOOP('',(#4978));
#1513=EDGE_LOOP('',(#4979));
#1514=EDGE_LOOP('',(#4980,#4981,#4982,#4983));
#1515=EDGE_LOOP('',(#4984));
#1516=EDGE_LOOP('',(#4985,#4986,#4987,#4988));
#1517=EDGE_LOOP('',(#4989,#4990,#4991,#4992));
#1518=EDGE_LOOP('',(#4993,#4994,#4995,#4996));
#1519=EDGE_LOOP('',(#4997,#4998,#4999,#5000));
#1520=EDGE_LOOP('',(#5001,#5002,#5003,#5004));
#1521=EDGE_LOOP('',(#5005,#5006,#5007,#5008));
#1522=EDGE_LOOP('',(#5009,#5010,#5011,#5012,#5013,#5014));
#1523=EDGE_LOOP('',(#5015,#5016,#5017,#5018,#5019,#5020));
#1524=EDGE_LOOP('',(#5021));
#1525=EDGE_LOOP('',(#5022));
#1526=EDGE_LOOP('',(#5023,#5024,#5025,#5026));
#1527=EDGE_LOOP('',(#5027,#5028,#5029,#5030));
#1528=EDGE_LOOP('',(#5031,#5032,#5033,#5034));
#1529=EDGE_LOOP('',(#5035));
#1530=EDGE_LOOP('',(#5036));
#1531=EDGE_LOOP('',(#5037,#5038,#5039,#5040));
#1532=EDGE_LOOP('',(#5041,#5042,#5043,#5044));
#1533=EDGE_LOOP('',(#5045,#5046,#5047,#5048,#5049,#5050));
#1534=EDGE_LOOP('',(#5051,#5052,#5053,#5054,#5055));
#1535=EDGE_LOOP('',(#5056,#5057,#5058,#5059));
#1536=EDGE_LOOP('',(#5060,#5061,#5062,#5063));
#1537=EDGE_LOOP('',(#5064));
#1538=EDGE_LOOP('',(#5065));
#1539=EDGE_LOOP('',(#5066,#5067,#5068,#5069,#5070));
#1540=EDGE_LOOP('',(#5071));
#1541=EDGE_LOOP('',(#5072));
#1542=EDGE_LOOP('',(#5073,#5074,#5075,#5076));
#1543=EDGE_LOOP('',(#5077,#5078,#5079,#5080,#5081,#5082));
#1544=EDGE_LOOP('',(#5083,#5084,#5085,#5086,#5087));
#1545=EDGE_LOOP('',(#5088));
#1546=EDGE_LOOP('',(#5089));
#1547=EDGE_LOOP('',(#5090,#5091,#5092,#5093));
#1548=EDGE_LOOP('',(#5094,#5095,#5096,#5097));
#1549=EDGE_LOOP('',(#5098,#5099,#5100,#5101));
#1550=EDGE_LOOP('',(#5102));
#1551=EDGE_LOOP('',(#5103));
#1552=EDGE_LOOP('',(#5104,#5105,#5106,#5107,#5108));
#1553=EDGE_LOOP('',(#5109,#5110));
#1554=EDGE_LOOP('',(#5111,#5112));
#1555=EDGE_LOOP('',(#5113,#5114));
#1556=EDGE_LOOP('',(#5115,#5116));
#1557=EDGE_LOOP('',(#5117,#5118));
#1558=EDGE_LOOP('',(#5119,#5120));
#1559=EDGE_LOOP('',(#5121,#5122));
#1560=EDGE_LOOP('',(#5123,#5124));
#1561=EDGE_LOOP('',(#5125,#5126,#5127,#5128));
#1562=EDGE_LOOP('',(#5129,#5130,#5131,#5132,#5133,#5134,#5135,#5136,#5137,
#5138,#5139,#5140,#5141,#5142,#5143,#5144,#5145,#5146,#5147,#5148));
#1563=EDGE_LOOP('',(#5149,#5150,#5151,#5152));
#1564=EDGE_LOOP('',(#5153,#5154,#5155,#5156));
#1565=EDGE_LOOP('',(#5157,#5158,#5159,#5160));
#1566=EDGE_LOOP('',(#5161,#5162,#5163,#5164));
#1567=EDGE_LOOP('',(#5165,#5166,#5167,#5168));
#1568=EDGE_LOOP('',(#5169,#5170,#5171,#5172,#5173,#5174));
#1569=EDGE_LOOP('',(#5175,#5176,#5177,#5178));
#1570=EDGE_LOOP('',(#5179,#5180,#5181,#5182));
#1571=EDGE_LOOP('',(#5183,#5184,#5185,#5186));
#1572=EDGE_LOOP('',(#5187,#5188,#5189,#5190));
#1573=EDGE_LOOP('',(#5191,#5192,#5193,#5194));
#1574=EDGE_LOOP('',(#5195,#5196,#5197,#5198));
#1575=EDGE_LOOP('',(#5199,#5200,#5201,#5202,#5203,#5204,#5205,#5206,#5207,
#5208,#5209,#5210,#5211,#5212,#5213,#5214,#5215,#5216,#5217,#5218));
#1576=EDGE_LOOP('',(#5219,#5220,#5221,#5222));
#1577=EDGE_LOOP('',(#5223,#5224,#5225,#5226));
#1578=EDGE_LOOP('',(#5227));
#1579=EDGE_LOOP('',(#5228));
#1580=EDGE_LOOP('',(#5229,#5230,#5231,#5232));
#1581=EDGE_LOOP('',(#5233));
#1582=EDGE_LOOP('',(#5234));
#1583=EDGE_LOOP('',(#5235,#5236,#5237,#5238));
#1584=EDGE_LOOP('',(#5239));
#1585=EDGE_LOOP('',(#5240));
#1586=EDGE_LOOP('',(#5241,#5242,#5243,#5244));
#1587=EDGE_LOOP('',(#5245));
#1588=EDGE_LOOP('',(#5246));
#1589=EDGE_LOOP('',(#5247,#5248,#5249,#5250));
#1590=EDGE_LOOP('',(#5251));
#1591=EDGE_LOOP('',(#5252));
#1592=EDGE_LOOP('',(#5253,#5254,#5255,#5256));
#1593=EDGE_LOOP('',(#5257,#5258,#5259,#5260));
#1594=EDGE_LOOP('',(#5261,#5262,#5263,#5264));
#1595=EDGE_LOOP('',(#5265,#5266,#5267,#5268));
#1596=EDGE_LOOP('',(#5269,#5270,#5271,#5272));
#1597=EDGE_LOOP('',(#5273,#5274,#5275,#5276));
#1598=EDGE_LOOP('',(#5277));
#1599=EDGE_LOOP('',(#5278));
#1600=EDGE_LOOP('',(#5279,#5280,#5281,#5282));
#1601=EDGE_LOOP('',(#5283));
#1602=EDGE_LOOP('',(#5284));
#1603=EDGE_LOOP('',(#5285,#5286,#5287,#5288));
#1604=EDGE_LOOP('',(#5289));
#1605=EDGE_LOOP('',(#5290));
#1606=EDGE_LOOP('',(#5291,#5292,#5293,#5294));
#1607=EDGE_LOOP('',(#5295));
#1608=EDGE_LOOP('',(#5296));
#1609=EDGE_LOOP('',(#5297,#5298,#5299,#5300));
#1610=EDGE_LOOP('',(#5301));
#1611=EDGE_LOOP('',(#5302));
#1612=EDGE_LOOP('',(#5303,#5304,#5305,#5306));
#1613=EDGE_LOOP('',(#5307));
#1614=EDGE_LOOP('',(#5308));
#1615=EDGE_LOOP('',(#5309,#5310,#5311,#5312));
#1616=EDGE_LOOP('',(#5313,#5314,#5315,#5316));
#1617=EDGE_LOOP('',(#5317,#5318,#5319,#5320));
#1618=EDGE_LOOP('',(#5321,#5322,#5323,#5324));
#1619=EDGE_LOOP('',(#5325,#5326,#5327,#5328));
#1620=EDGE_LOOP('',(#5329,#5330,#5331,#5332));
#1621=EDGE_LOOP('',(#5333));
#1622=EDGE_LOOP('',(#5334));
#1623=EDGE_LOOP('',(#5335,#5336,#5337,#5338));
#1624=EDGE_LOOP('',(#5339,#5340,#5341,#5342));
#1625=EDGE_LOOP('',(#5343));
#1626=EDGE_LOOP('',(#5344));
#1627=EDGE_LOOP('',(#5345,#5346,#5347,#5348));
#1628=EDGE_LOOP('',(#5349,#5350,#5351,#5352));
#1629=EDGE_LOOP('',(#5353,#5354,#5355,#5356));
#1630=EDGE_LOOP('',(#5357,#5358,#5359,#5360));
#1631=EDGE_LOOP('',(#5361,#5362,#5363,#5364));
#1632=EDGE_LOOP('',(#5365,#5366,#5367,#5368));
#1633=EDGE_LOOP('',(#5369,#5370,#5371,#5372));
#1634=EDGE_LOOP('',(#5373,#5374,#5375,#5376));
#1635=EDGE_LOOP('',(#5377,#5378,#5379,#5380,#5381,#5382));
#1636=EDGE_LOOP('',(#5383,#5384,#5385,#5386,#5387,#5388));
#1637=EDGE_LOOP('',(#5389));
#1638=EDGE_LOOP('',(#5390));
#1639=EDGE_LOOP('',(#5391,#5392,#5393,#5394));
#1640=EDGE_LOOP('',(#5395));
#1641=EDGE_LOOP('',(#5396));
#1642=EDGE_LOOP('',(#5397,#5398,#5399,#5400));
#1643=EDGE_LOOP('',(#5401,#5402,#5403,#5404));
#1644=EDGE_LOOP('',(#5405,#5406,#5407,#5408));
#1645=EDGE_LOOP('',(#5409));
#1646=EDGE_LOOP('',(#5410));
#1647=EDGE_LOOP('',(#5411,#5412,#5413,#5414));
#1648=EDGE_LOOP('',(#5415,#5416,#5417,#5418));
#1649=EDGE_LOOP('',(#5419,#5420,#5421,#5422));
#1650=EDGE_LOOP('',(#5423,#5424,#5425,#5426));
#1651=EDGE_LOOP('',(#5427,#5428,#5429,#5430));
#1652=EDGE_LOOP('',(#5431,#5432,#5433,#5434,#5435,#5436,#5437,#5438,#5439));
#1653=EDGE_LOOP('',(#5440));
#1654=EDGE_LOOP('',(#5441));
#1655=EDGE_LOOP('',(#5442,#5443,#5444,#5445));
#1656=EDGE_LOOP('',(#5446,#5447,#5448,#5449));
#1657=EDGE_LOOP('',(#5450,#5451,#5452,#5453));
#1658=EDGE_LOOP('',(#5454,#5455,#5456,#5457));
#1659=EDGE_LOOP('',(#5458,#5459,#5460,#5461));
#1660=EDGE_LOOP('',(#5462,#5463,#5464,#5465));
#1661=EDGE_LOOP('',(#5466));
#1662=EDGE_LOOP('',(#5467,#5468,#5469,#5470));
#1663=EDGE_LOOP('',(#5471));
#1664=EDGE_LOOP('',(#5472));
#1665=EDGE_LOOP('',(#5473,#5474,#5475,#5476,#5477,#5478,#5479,#5480,#5481,
#5482,#5483,#5484));
#1666=EDGE_LOOP('',(#5485));
#1667=EDGE_LOOP('',(#5486));
#1668=EDGE_LOOP('',(#5487,#5488,#5489,#5490));
#1669=EDGE_LOOP('',(#5491,#5492,#5493,#5494));
#1670=EDGE_LOOP('',(#5495,#5496,#5497,#5498));
#1671=EDGE_LOOP('',(#5499));
#1672=EDGE_LOOP('',(#5500));
#1673=EDGE_LOOP('',(#5501,#5502,#5503,#5504));
#1674=EDGE_LOOP('',(#5505,#5506,#5507,#5508));
#1675=EDGE_LOOP('',(#5509));
#1676=EDGE_LOOP('',(#5510));
#1677=EDGE_LOOP('',(#5511));
#1678=EDGE_LOOP('',(#5512));
#1679=EDGE_LOOP('',(#5513,#5514));
#1680=EDGE_LOOP('',(#5515,#5516,#5517,#5518,#5519,#5520,#5521,#5522,#5523));
#1681=EDGE_LOOP('',(#5524,#5525,#5526));
#1682=EDGE_LOOP('',(#5527,#5528,#5529,#5530));
#1683=EDGE_LOOP('',(#5531,#5532,#5533,#5534));
#1684=EDGE_LOOP('',(#5535,#5536,#5537,#5538));
#1685=EDGE_LOOP('',(#5539,#5540));
#1686=EDGE_LOOP('',(#5541));
#1687=EDGE_LOOP('',(#5542));
#1688=EDGE_LOOP('',(#5543));
#1689=EDGE_LOOP('',(#5544));
#1690=EDGE_LOOP('',(#5545,#5546,#5547,#5548));
#1691=EDGE_LOOP('',(#5549));
#1692=EDGE_LOOP('',(#5550,#5551,#5552,#5553));
#1693=EDGE_LOOP('',(#5554));
#1694=EDGE_LOOP('',(#5555));
#1695=EDGE_LOOP('',(#5556));
#1696=EDGE_LOOP('',(#5557));
#1697=EDGE_LOOP('',(#5558));
#1698=EDGE_LOOP('',(#5559,#5560,#5561,#5562));
#1699=EDGE_LOOP('',(#5563,#5564,#5565,#5566));
#1700=EDGE_LOOP('',(#5567,#5568,#5569,#5570));
#1701=EDGE_LOOP('',(#5571));
#1702=EDGE_LOOP('',(#5572));
#1703=EDGE_LOOP('',(#5573));
#1704=EDGE_LOOP('',(#5574));
#1705=EDGE_LOOP('',(#5575,#5576,#5577,#5578));
#1706=EDGE_LOOP('',(#5579,#5580,#5581,#5582));
#1707=EDGE_LOOP('',(#5583));
#1708=EDGE_LOOP('',(#5584));
#1709=EDGE_LOOP('',(#5585));
#1710=EDGE_LOOP('',(#5586));
#1711=EDGE_LOOP('',(#5587,#5588,#5589,#5590));
#1712=EDGE_LOOP('',(#5591,#5592,#5593,#5594));
#1713=EDGE_LOOP('',(#5595));
#1714=EDGE_LOOP('',(#5596));
#1715=EDGE_LOOP('',(#5597));
#1716=EDGE_LOOP('',(#5598));
#1717=EDGE_LOOP('',(#5599,#5600,#5601,#5602));
#1718=EDGE_LOOP('',(#5603,#5604,#5605,#5606));
#1719=EDGE_LOOP('',(#5607));
#1720=EDGE_LOOP('',(#5608));
#1721=EDGE_LOOP('',(#5609));
#1722=EDGE_LOOP('',(#5610));
#1723=EDGE_LOOP('',(#5611,#5612,#5613,#5614));
#1724=EDGE_LOOP('',(#5615,#5616,#5617,#5618));
#1725=EDGE_LOOP('',(#5619));
#1726=EDGE_LOOP('',(#5620));
#1727=EDGE_LOOP('',(#5621));
#1728=EDGE_LOOP('',(#5622));
#1729=EDGE_LOOP('',(#5623));
#1730=EDGE_LOOP('',(#5624,#5625,#5626,#5627));
#1731=EDGE_LOOP('',(#5628,#5629,#5630,#5631));
#1732=EDGE_LOOP('',(#5632,#5633,#5634,#5635));
#1733=EDGE_LOOP('',(#5636,#5637,#5638,#5639));
#1734=EDGE_LOOP('',(#5640,#5641,#5642,#5643));
#1735=EDGE_LOOP('',(#5644,#5645,#5646,#5647));
#1736=EDGE_LOOP('',(#5648,#5649,#5650,#5651,#5652,#5653));
#1737=EDGE_LOOP('',(#5654));
#1738=EDGE_LOOP('',(#5655,#5656,#5657,#5658,#5659,#5660));
#1739=EDGE_LOOP('',(#5661,#5662,#5663,#5664));
#1740=EDGE_LOOP('',(#5665,#5666,#5667,#5668));
#1741=EDGE_LOOP('',(#5669,#5670,#5671,#5672));
#1742=EDGE_LOOP('',(#5673,#5674,#5675,#5676));
#1743=EDGE_LOOP('',(#5677,#5678,#5679,#5680));
#1744=EDGE_LOOP('',(#5681,#5682,#5683,#5684));
#1745=EDGE_LOOP('',(#5685,#5686,#5687,#5688));
#1746=EDGE_LOOP('',(#5689,#5690,#5691,#5692));
#1747=EDGE_LOOP('',(#5693,#5694,#5695,#5696,#5697,#5698));
#1748=EDGE_LOOP('',(#5699,#5700,#5701,#5702,#5703,#5704));
#1749=EDGE_LOOP('',(#5705));
#1750=EDGE_LOOP('',(#5706));
#1751=EDGE_LOOP('',(#5707,#5708,#5709,#5710));
#1752=EDGE_LOOP('',(#5711,#5712,#5713,#5714));
#1753=EDGE_LOOP('',(#5715,#5716,#5717,#5718));
#1754=EDGE_LOOP('',(#5719));
#1755=EDGE_LOOP('',(#5720));
#1756=EDGE_LOOP('',(#5721,#5722,#5723,#5724));
#1757=EDGE_LOOP('',(#5725,#5726,#5727,#5728));
#1758=EDGE_LOOP('',(#5729));
#1759=EDGE_LOOP('',(#5730,#5731,#5732,#5733));
#1760=EDGE_LOOP('',(#5734,#5735,#5736,#5737));
#1761=EDGE_LOOP('',(#5738,#5739,#5740,#5741));
#1762=EDGE_LOOP('',(#5742));
#1763=EDGE_LOOP('',(#5743));
#1764=EDGE_LOOP('',(#5744,#5745,#5746,#5747));
#1765=EDGE_LOOP('',(#5748,#5749,#5750,#5751));
#1766=EDGE_LOOP('',(#5752,#5753,#5754,#5755));
#1767=EDGE_LOOP('',(#5756));
#1768=EDGE_LOOP('',(#5757,#5758,#5759,#5760));
#1769=EDGE_LOOP('',(#5761,#5762,#5763,#5764));
#1770=EDGE_LOOP('',(#5765,#5766,#5767,#5768));
#1771=EDGE_LOOP('',(#5769,#5770,#5771,#5772));
#1772=EDGE_LOOP('',(#5773,#5774,#5775,#5776));
#1773=EDGE_LOOP('',(#5777,#5778,#5779,#5780));
#1774=EDGE_LOOP('',(#5781,#5782,#5783,#5784,#5785,#5786));
#1775=EDGE_LOOP('',(#5787,#5788,#5789,#5790,#5791,#5792));
#1776=EDGE_LOOP('',(#5793,#5794,#5795,#5796));
#1777=EDGE_LOOP('',(#5797,#5798,#5799,#5800));
#1778=EDGE_LOOP('',(#5801,#5802,#5803,#5804));
#1779=EDGE_LOOP('',(#5805,#5806,#5807,#5808));
#1780=EDGE_LOOP('',(#5809,#5810,#5811,#5812));
#1781=EDGE_LOOP('',(#5813));
#1782=EDGE_LOOP('',(#5814));
#1783=EDGE_LOOP('',(#5815,#5816,#5817,#5818));
#1784=EDGE_LOOP('',(#5819,#5820,#5821,#5822));
#1785=EDGE_LOOP('',(#5823,#5824,#5825,#5826));
#1786=EDGE_LOOP('',(#5827));
#1787=EDGE_LOOP('',(#5828));
#1788=EDGE_LOOP('',(#5829,#5830,#5831,#5832));
#1789=EDGE_LOOP('',(#5833,#5834,#5835,#5836));
#1790=EDGE_LOOP('',(#5837));
#1791=EDGE_LOOP('',(#5838));
#1792=EDGE_LOOP('',(#5839));
#1793=EDGE_LOOP('',(#5840));
#1794=EDGE_LOOP('',(#5841,#5842,#5843,#5844));
#1795=EDGE_LOOP('',(#5845,#5846,#5847,#5848));
#1796=EDGE_LOOP('',(#5849));
#1797=EDGE_LOOP('',(#5850));
#1798=EDGE_LOOP('',(#5851));
#1799=EDGE_LOOP('',(#5852));
#1800=EDGE_LOOP('',(#5853,#5854,#5855,#5856));
#1801=EDGE_LOOP('',(#5857));
#1802=EDGE_LOOP('',(#5858,#5859,#5860,#5861));
#1803=EDGE_LOOP('',(#5862));
#1804=EDGE_LOOP('',(#5863,#5864,#5865,#5866,#5867,#5868));
#1805=EDGE_LOOP('',(#5869,#5870,#5871,#5872));
#1806=EDGE_LOOP('',(#5873,#5874,#5875,#5876,#5877,#5878));
#1807=EDGE_LOOP('',(#5879,#5880,#5881,#5882));
#1808=EDGE_LOOP('',(#5883,#5884,#5885,#5886));
#1809=EDGE_LOOP('',(#5887,#5888,#5889,#5890,#5891,#5892));
#1810=EDGE_LOOP('',(#5893,#5894,#5895,#5896,#5897,#5898,#5899));
#1811=EDGE_LOOP('',(#5900,#5901,#5902,#5903,#5904,#5905,#5906));
#1812=EDGE_LOOP('',(#5907,#5908,#5909,#5910,#5911,#5912,#5913,#5914));
#1813=EDGE_LOOP('',(#5915));
#1814=EDGE_LOOP('',(#5916));
#1815=EDGE_LOOP('',(#5917,#5918));
#1816=EDGE_LOOP('',(#5919,#5920,#5921,#5922,#5923,#5924,#5925,#5926));
#1817=EDGE_LOOP('',(#5927,#5928,#5929));
#1818=EDGE_LOOP('',(#5930,#5931,#5932,#5933));
#1819=EDGE_LOOP('',(#5934,#5935,#5936,#5937));
#1820=EDGE_LOOP('',(#5938,#5939,#5940,#5941));
#1821=EDGE_LOOP('',(#5942));
#1822=EDGE_LOOP('',(#5943,#5944,#5945,#5946));
#1823=EDGE_LOOP('',(#5947,#5948,#5949,#5950));
#1824=EDGE_LOOP('',(#5951,#5952,#5953,#5954));
#1825=EDGE_LOOP('',(#5955,#5956,#5957,#5958));
#1826=EDGE_LOOP('',(#5959));
#1827=EDGE_LOOP('',(#5960,#5961,#5962,#5963));
#1828=EDGE_LOOP('',(#5964));
#1829=EDGE_LOOP('',(#5965));
#1830=EDGE_LOOP('',(#5966));
#1831=EDGE_LOOP('',(#5967,#5968,#5969,#5970));
#1832=EDGE_LOOP('',(#5971));
#1833=EDGE_LOOP('',(#5972,#5973,#5974,#5975));
#1834=EDGE_LOOP('',(#5976));
#1835=EDGE_LOOP('',(#5977,#5978,#5979,#5980));
#1836=EDGE_LOOP('',(#5981));
#1837=EDGE_LOOP('',(#5982));
#1838=EDGE_LOOP('',(#5983,#5984,#5985,#5986));
#1839=EDGE_LOOP('',(#5987,#5988,#5989,#5990));
#1840=EDGE_LOOP('',(#5991,#5992,#5993,#5994));
#1841=EDGE_LOOP('',(#5995,#5996,#5997,#5998));
#1842=EDGE_LOOP('',(#5999,#6000,#6001,#6002));
#1843=EDGE_LOOP('',(#6003,#6004,#6005,#6006));
#1844=EDGE_LOOP('',(#6007,#6008,#6009,#6010,#6011,#6012));
#1845=EDGE_LOOP('',(#6013));
#1846=EDGE_LOOP('',(#6014,#6015,#6016,#6017,#6018,#6019));
#1847=EDGE_LOOP('',(#6020,#6021,#6022,#6023));
#1848=EDGE_LOOP('',(#6024,#6025,#6026,#6027));
#1849=EDGE_LOOP('',(#6028,#6029,#6030,#6031));
#1850=EDGE_LOOP('',(#6032));
#1851=LINE('',#10052,#2292);
#1852=LINE('',#10058,#2293);
#1853=LINE('',#10064,#2294);
#1854=LINE('',#10070,#2295);
#1855=LINE('',#10076,#2296);
#1856=LINE('',#10082,#2297);
#1857=LINE('',#10088,#2298);
#1858=LINE('',#10094,#2299);
#1859=LINE('',#10099,#2300);
#1860=LINE('',#10101,#2301);
#1861=LINE('',#10103,#2302);
#1862=LINE('',#10104,#2303);
#1863=LINE('',#10107,#2304);
#1864=LINE('',#10109,#2305);
#1865=LINE('',#10110,#2306);
#1866=LINE('',#10113,#2307);
#1867=LINE('',#10115,#2308);
#1868=LINE('',#10116,#2309);
#1869=LINE('',#10118,#2310);
#1870=LINE('',#10119,#2311);
#1871=LINE('',#10126,#2312);
#1872=LINE('',#10128,#2313);
#1873=LINE('',#10130,#2314);
#1874=LINE('',#10131,#2315);
#1875=LINE('',#10134,#2316);
#1876=LINE('',#10136,#2317);
#1877=LINE('',#10137,#2318);
#1878=LINE('',#10140,#2319);
#1879=LINE('',#10142,#2320);
#1880=LINE('',#10143,#2321);
#1881=LINE('',#10145,#2322);
#1882=LINE('',#10146,#2323);
#1883=LINE('',#10153,#2324);
#1884=LINE('',#10155,#2325);
#1885=LINE('',#10157,#2326);
#1886=LINE('',#10158,#2327);
#1887=LINE('',#10161,#2328);
#1888=LINE('',#10163,#2329);
#1889=LINE('',#10164,#2330);
#1890=LINE('',#10167,#2331);
#1891=LINE('',#10169,#2332);
#1892=LINE('',#10170,#2333);
#1893=LINE('',#10172,#2334);
#1894=LINE('',#10173,#2335);
#1895=LINE('',#10181,#2336);
#1896=LINE('',#10187,#2337);
#1897=LINE('',#10194,#2338);
#1898=LINE('',#10201,#2339);
#1899=LINE('',#10208,#2340);
#1900=LINE('',#10215,#2341);
#1901=LINE('',#10221,#2342);
#1902=LINE('',#10227,#2343);
#1903=LINE('',#10233,#2344);
#1904=LINE('',#10239,#2345);
#1905=LINE('',#10245,#2346);
#1906=LINE('',#10251,#2347);
#1907=LINE('',#10257,#2348);
#1908=LINE('',#10263,#2349);
#1909=LINE('',#10271,#2350);
#1910=LINE('',#10276,#2351);
#1911=LINE('',#10281,#2352);
#1912=LINE('',#10285,#2353);
#1913=LINE('',#10289,#2354);
#1914=LINE('',#10291,#2355);
#1915=LINE('',#10293,#2356);
#1916=LINE('',#10295,#2357);
#1917=LINE('',#10297,#2358);
#1918=LINE('',#10299,#2359);
#1919=LINE('',#10301,#2360);
#1920=LINE('',#10304,#2361);
#1921=LINE('',#10307,#2362);
#1922=LINE('',#10308,#2363);
#1923=LINE('',#10312,#2364);
#1924=LINE('',#10314,#2365);
#1925=LINE('',#10316,#2366);
#1926=LINE('',#10317,#2367);
#1927=LINE('',#10320,#2368);
#1928=LINE('',#10321,#2369);
#1929=LINE('',#10322,#2370);
#1930=LINE('',#10326,#2371);
#1931=LINE('',#10327,#2372);
#1932=LINE('',#10328,#2373);
#1933=LINE('',#10331,#2374);
#1934=LINE('',#10332,#2375);
#1935=LINE('',#10335,#2376);
#1936=LINE('',#10336,#2377);
#1937=LINE('',#10338,#2378);
#1938=LINE('',#10341,#2379);
#1939=LINE('',#10342,#2380);
#1940=LINE('',#10345,#2381);
#1941=LINE('',#10347,#2382);
#1942=LINE('',#10350,#2383);
#1943=LINE('',#10351,#2384);
#1944=LINE('',#10353,#2385);
#1945=LINE('',#10355,#2386);
#1946=LINE('',#10356,#2387);
#1947=LINE('',#10360,#2388);
#1948=LINE('',#10362,#2389);
#1949=LINE('',#10370,#2390);
#1950=LINE('',#10376,#2391);
#1951=LINE('',#10382,#2392);
#1952=LINE('',#10388,#2393);
#1953=LINE('',#10394,#2394);
#1954=LINE('',#10401,#2395);
#1955=LINE('',#10407,#2396);
#1956=LINE('',#10416,#2397);
#1957=LINE('',#10422,#2398);
#1958=LINE('',#10428,#2399);
#1959=LINE('',#10434,#2400);
#1960=LINE('',#10440,#2401);
#1961=LINE('',#10448,#2402);
#1962=LINE('',#10453,#2403);
#1963=LINE('',#10462,#2404);
#1964=LINE('',#10471,#2405);
#1965=LINE('',#10480,#2406);
#1966=LINE('',#10489,#2407);
#1967=LINE('',#10497,#2408);
#1968=LINE('',#10501,#2409);
#1969=LINE('',#10505,#2410);
#1970=LINE('',#10509,#2411);
#1971=LINE('',#10514,#2412);
#1972=LINE('',#10522,#2413);
#1973=LINE('',#10527,#2414);
#1974=LINE('',#10535,#2415);
#1975=LINE('',#10537,#2416);
#1976=LINE('',#10539,#2417);
#1977=LINE('',#10540,#2418);
#1978=LINE('',#10543,#2419);
#1979=LINE('',#10545,#2420);
#1980=LINE('',#10546,#2421);
#1981=LINE('',#10549,#2422);
#1982=LINE('',#10551,#2423);
#1983=LINE('',#10552,#2424);
#1984=LINE('',#10554,#2425);
#1985=LINE('',#10555,#2426);
#1986=LINE('',#10563,#2427);
#1987=LINE('',#10570,#2428);
#1988=LINE('',#10576,#2429);
#1989=LINE('',#10578,#2430);
#1990=LINE('',#10580,#2431);
#1991=LINE('',#10581,#2432);
#1992=LINE('',#10584,#2433);
#1993=LINE('',#10586,#2434);
#1994=LINE('',#10587,#2435);
#1995=LINE('',#10590,#2436);
#1996=LINE('',#10592,#2437);
#1997=LINE('',#10593,#2438);
#1998=LINE('',#10595,#2439);
#1999=LINE('',#10596,#2440);
#2000=LINE('',#10604,#2441);
#2001=LINE('',#10611,#2442);
#2002=LINE('',#10617,#2443);
#2003=LINE('',#10619,#2444);
#2004=LINE('',#10621,#2445);
#2005=LINE('',#10622,#2446);
#2006=LINE('',#10625,#2447);
#2007=LINE('',#10627,#2448);
#2008=LINE('',#10628,#2449);
#2009=LINE('',#10631,#2450);
#2010=LINE('',#10633,#2451);
#2011=LINE('',#10634,#2452);
#2012=LINE('',#10636,#2453);
#2013=LINE('',#10637,#2454);
#2014=LINE('',#10645,#2455);
#2015=LINE('',#10656,#2456);
#2016=LINE('',#10660,#2457);
#2017=LINE('',#10667,#2458);
#2018=LINE('',#10669,#2459);
#2019=LINE('',#10671,#2460);
#2020=LINE('',#10672,#2461);
#2021=LINE('',#10675,#2462);
#2022=LINE('',#10677,#2463);
#2023=LINE('',#10678,#2464);
#2024=LINE('',#10681,#2465);
#2025=LINE('',#10683,#2466);
#2026=LINE('',#10684,#2467);
#2027=LINE('',#10687,#2468);
#2028=LINE('',#10689,#2469);
#2029=LINE('',#10690,#2470);
#2030=LINE('',#10693,#2471);
#2031=LINE('',#10695,#2472);
#2032=LINE('',#10696,#2473);
#2033=LINE('',#10698,#2474);
#2034=LINE('',#10699,#2475);
#2035=LINE('',#10711,#2476);
#2036=LINE('',#10715,#2477);
#2037=LINE('',#10719,#2478);
#2038=LINE('',#10726,#2479);
#2039=LINE('',#10728,#2480);
#2040=LINE('',#10743,#2481);
#2041=LINE('',#10749,#2482);
#2042=LINE('',#10753,#2483);
#2043=LINE('',#10759,#2484);
#2044=LINE('',#10764,#2485);
#2045=LINE('',#10779,#2486);
#2046=LINE('',#10788,#2487);
#2047=LINE('',#10792,#2488);
#2048=LINE('',#10796,#2489);
#2049=LINE('',#10799,#2490);
#2050=LINE('',#10952,#2491);
#2051=LINE('',#11248,#2492);
#2052=LINE('',#11290,#2493);
#2053=LINE('',#11295,#2494);
#2054=LINE('',#11304,#2495);
#2055=LINE('',#11309,#2496);
#2056=LINE('',#11322,#2497);
#2057=LINE('',#11324,#2498);
#2058=LINE('',#11325,#2499);
#2059=LINE('',#11328,#2500);
#2060=LINE('',#11330,#2501);
#2061=LINE('',#11331,#2502);
#2062=LINE('',#11336,#2503);
#2063=LINE('',#11337,#2504);
#2064=LINE('',#11339,#2505);
#2065=LINE('',#11340,#2506);
#2066=LINE('',#11350,#2507);
#2067=LINE('',#11357,#2508);
#2068=LINE('',#11364,#2509);
#2069=LINE('',#11371,#2510);
#2070=LINE('',#11378,#2511);
#2071=LINE('',#11383,#2512);
#2072=LINE('',#11390,#2513);
#2073=LINE('',#11393,#2514);
#2074=LINE('',#11396,#2515);
#2075=LINE('',#11398,#2516);
#2076=LINE('',#11399,#2517);
#2077=LINE('',#11405,#2518);
#2078=LINE('',#11407,#2519);
#2079=LINE('',#11408,#2520);
#2080=LINE('',#11417,#2521);
#2081=LINE('',#11422,#2522);
#2082=LINE('',#11429,#2523);
#2083=LINE('',#11431,#2524);
#2084=LINE('',#11433,#2525);
#2085=LINE('',#11434,#2526);
#2086=LINE('',#11437,#2527);
#2087=LINE('',#11439,#2528);
#2088=LINE('',#11440,#2529);
#2089=LINE('',#11443,#2530);
#2090=LINE('',#11445,#2531);
#2091=LINE('',#11446,#2532);
#2092=LINE('',#11449,#2533);
#2093=LINE('',#11451,#2534);
#2094=LINE('',#11452,#2535);
#2095=LINE('',#11455,#2536);
#2096=LINE('',#11457,#2537);
#2097=LINE('',#11458,#2538);
#2098=LINE('',#11460,#2539);
#2099=LINE('',#11461,#2540);
#2100=LINE('',#11471,#2541);
#2101=LINE('',#11480,#2542);
#2102=LINE('',#11484,#2543);
#2103=LINE('',#11488,#2544);
#2104=LINE('',#11495,#2545);
#2105=LINE('',#11499,#2546);
#2106=LINE('',#11501,#2547);
#2107=LINE('',#11508,#2548);
#2108=LINE('',#11513,#2549);
#2109=LINE('',#11517,#2550);
#2110=LINE('',#11521,#2551);
#2111=LINE('',#11527,#2552);
#2112=LINE('',#11531,#2553);
#2113=LINE('',#11534,#2554);
#2114=LINE('',#11539,#2555);
#2115=LINE('',#11540,#2556);
#2116=LINE('',#11543,#2557);
#2117=LINE('',#11546,#2558);
#2118=LINE('',#11549,#2559);
#2119=LINE('',#11552,#2560);
#2120=LINE('',#11555,#2561);
#2121=LINE('',#11556,#2562);
#2122=LINE('',#11559,#2563);
#2123=LINE('',#11562,#2564);
#2124=LINE('',#11569,#2565);
#2125=LINE('',#11576,#2566);
#2126=LINE('',#11579,#2567);
#2127=LINE('',#11584,#2568);
#2128=LINE('',#11592,#2569);
#2129=LINE('',#11598,#2570);
#2130=LINE('',#11606,#2571);
#2131=LINE('',#11627,#2572);
#2132=LINE('',#11682,#2573);
#2133=LINE('',#11687,#2574);
#2134=LINE('',#11693,#2575);
#2135=LINE('',#11702,#2576);
#2136=LINE('',#11709,#2577);
#2137=LINE('',#11723,#2578);
#2138=LINE('',#11726,#2579);
#2139=LINE('',#11731,#2580);
#2140=LINE('',#11739,#2581);
#2141=LINE('',#11745,#2582);
#2142=LINE('',#11754,#2583);
#2143=LINE('',#11760,#2584);
#2144=LINE('',#11769,#2585);
#2145=LINE('',#11775,#2586);
#2146=LINE('',#11784,#2587);
#2147=LINE('',#11790,#2588);
#2148=LINE('',#11801,#2589);
#2149=LINE('',#11803,#2590);
#2150=LINE('',#11805,#2591);
#2151=LINE('',#11806,#2592);
#2152=LINE('',#11809,#2593);
#2153=LINE('',#11811,#2594);
#2154=LINE('',#11812,#2595);
#2155=LINE('',#11815,#2596);
#2156=LINE('',#11817,#2597);
#2157=LINE('',#11818,#2598);
#2158=LINE('',#11821,#2599);
#2159=LINE('',#11823,#2600);
#2160=LINE('',#11824,#2601);
#2161=LINE('',#11827,#2602);
#2162=LINE('',#11829,#2603);
#2163=LINE('',#11830,#2604);
#2164=LINE('',#11832,#2605);
#2165=LINE('',#11833,#2606);
#2166=LINE('',#11841,#2607);
#2167=LINE('',#11843,#2608);
#2168=LINE('',#11848,#2609);
#2169=LINE('',#11850,#2610);
#2170=LINE('',#11852,#2611);
#2171=LINE('',#11853,#2612);
#2172=LINE('',#11856,#2613);
#2173=LINE('',#11858,#2614);
#2174=LINE('',#11859,#2615);
#2175=LINE('',#11862,#2616);
#2176=LINE('',#11864,#2617);
#2177=LINE('',#11865,#2618);
#2178=LINE('',#11868,#2619);
#2179=LINE('',#11870,#2620);
#2180=LINE('',#11871,#2621);
#2181=LINE('',#11874,#2622);
#2182=LINE('',#11876,#2623);
#2183=LINE('',#11877,#2624);
#2184=LINE('',#11879,#2625);
#2185=LINE('',#11880,#2626);
#2186=LINE('',#11892,#2627);
#2187=LINE('',#11896,#2628);
#2188=LINE('',#11900,#2629);
#2189=LINE('',#11907,#2630);
#2190=LINE('',#11909,#2631);
#2191=LINE('',#11917,#2632);
#2192=LINE('',#11921,#2633);
#2193=LINE('',#11925,#2634);
#2194=LINE('',#11932,#2635);
#2195=LINE('',#11936,#2636);
#2196=LINE('',#11940,#2637);
#2197=LINE('',#11945,#2638);
#2198=LINE('',#11947,#2639);
#2199=LINE('',#11949,#2640);
#2200=LINE('',#11950,#2641);
#2201=LINE('',#11953,#2642);
#2202=LINE('',#11955,#2643);
#2203=LINE('',#11956,#2644);
#2204=LINE('',#11959,#2645);
#2205=LINE('',#11961,#2646);
#2206=LINE('',#11962,#2647);
#2207=LINE('',#11965,#2648);
#2208=LINE('',#11967,#2649);
#2209=LINE('',#11968,#2650);
#2210=LINE('',#11971,#2651);
#2211=LINE('',#11973,#2652);
#2212=LINE('',#11974,#2653);
#2213=LINE('',#11976,#2654);
#2214=LINE('',#11977,#2655);
#2215=LINE('',#12031,#2656);
#2216=LINE('',#12037,#2657);
#2217=LINE('',#12042,#2658);
#2218=LINE('',#12046,#2659);
#2219=LINE('',#12050,#2660);
#2220=LINE('',#12052,#2661);
#2221=LINE('',#12053,#2662);
#2222=LINE('',#12056,#2663);
#2223=LINE('',#12060,#2664);
#2224=LINE('',#12061,#2665);
#2225=LINE('',#12070,#2666);
#2226=LINE('',#12076,#2667);
#2227=LINE('',#12085,#2668);
#2228=LINE('',#12091,#2669);
#2229=LINE('',#12104,#2670);
#2230=LINE('',#12110,#2671);
#2231=LINE('',#12112,#2672);
#2232=LINE('',#12114,#2673);
#2233=LINE('',#12115,#2674);
#2234=LINE('',#12118,#2675);
#2235=LINE('',#12120,#2676);
#2236=LINE('',#12122,#2677);
#2237=LINE('',#12124,#2678);
#2238=LINE('',#12125,#2679);
#2239=LINE('',#12128,#2680);
#2240=LINE('',#12132,#2681);
#2241=LINE('',#12134,#2682);
#2242=LINE('',#12136,#2683);
#2243=LINE('',#12137,#2684);
#2244=LINE('',#12141,#2685);
#2245=LINE('',#12142,#2686);
#2246=LINE('',#12143,#2687);
#2247=LINE('',#12146,#2688);
#2248=LINE('',#12148,#2689);
#2249=LINE('',#12149,#2690);
#2250=LINE('',#12155,#2691);
#2251=LINE('',#12163,#2692);
#2252=LINE('',#12170,#2693);
#2253=LINE('',#12187,#2694);
#2254=LINE('',#12202,#2695);
#2255=LINE('',#12207,#2696);
#2256=LINE('',#12212,#2697);
#2257=LINE('',#12214,#2698);
#2258=LINE('',#12216,#2699);
#2259=LINE('',#12217,#2700);
#2260=LINE('',#12221,#2701);
#2261=LINE('',#12222,#2702);
#2262=LINE('',#12223,#2703);
#2263=LINE('',#12226,#2704);
#2264=LINE('',#12227,#2705);
#2265=LINE('',#12230,#2706);
#2266=LINE('',#12231,#2707);
#2267=LINE('',#12233,#2708);
#2268=LINE('',#12243,#2709);
#2269=LINE('',#12249,#2710);
#2270=LINE('',#12256,#2711);
#2271=LINE('',#12264,#2712);
#2272=LINE('',#12266,#2713);
#2273=LINE('',#12268,#2714);
#2274=LINE('',#12269,#2715);
#2275=LINE('',#12272,#2716);
#2276=LINE('',#12274,#2717);
#2277=LINE('',#12275,#2718);
#2278=LINE('',#12278,#2719);
#2279=LINE('',#12280,#2720);
#2280=LINE('',#12281,#2721);
#2281=LINE('',#12284,#2722);
#2282=LINE('',#12286,#2723);
#2283=LINE('',#12287,#2724);
#2284=LINE('',#12290,#2725);
#2285=LINE('',#12292,#2726);
#2286=LINE('',#12293,#2727);
#2287=LINE('',#12295,#2728);
#2288=LINE('',#12296,#2729);
#2289=LINE('',#12304,#2730);
#2290=LINE('',#12308,#2731);
#2291=LINE('',#12312,#2732);
#2292=VECTOR('',#7904,0.225);
#2293=VECTOR('',#7911,0.225);
#2294=VECTOR('',#7918,0.225);
#2295=VECTOR('',#7925,0.225);
#2296=VECTOR('',#7932,0.21);
#2297=VECTOR('',#7939,0.210000000000001);
#2298=VECTOR('',#7946,0.210000000000001);
#2299=VECTOR('',#7953,0.21);
#2300=VECTOR('',#7958,1.);
#2301=VECTOR('',#7959,1.);
#2302=VECTOR('',#7960,1.);
#2303=VECTOR('',#7961,1.);
#2304=VECTOR('',#7964,1.);
#2305=VECTOR('',#7965,1.);
#2306=VECTOR('',#7966,1.);
#2307=VECTOR('',#7969,1.);
#2308=VECTOR('',#7970,1.);
#2309=VECTOR('',#7971,1.);
#2310=VECTOR('',#7974,1.);
#2311=VECTOR('',#7975,1.);
#2312=VECTOR('',#7984,1.);
#2313=VECTOR('',#7985,1.);
#2314=VECTOR('',#7986,1.);
#2315=VECTOR('',#7987,1.);
#2316=VECTOR('',#7990,1.);
#2317=VECTOR('',#7991,1.);
#2318=VECTOR('',#7992,1.);
#2319=VECTOR('',#7995,1.);
#2320=VECTOR('',#7996,1.);
#2321=VECTOR('',#7997,1.);
#2322=VECTOR('',#8000,1.);
#2323=VECTOR('',#8001,1.);
#2324=VECTOR('',#8010,1.);
#2325=VECTOR('',#8011,1.);
#2326=VECTOR('',#8012,1.);
#2327=VECTOR('',#8013,1.);
#2328=VECTOR('',#8016,1.);
#2329=VECTOR('',#8017,1.);
#2330=VECTOR('',#8018,1.);
#2331=VECTOR('',#8021,1.);
#2332=VECTOR('',#8022,1.);
#2333=VECTOR('',#8023,1.);
#2334=VECTOR('',#8026,1.);
#2335=VECTOR('',#8027,1.);
#2336=VECTOR('',#8038,0.225);
#2337=VECTOR('',#8045,0.165);
#2338=VECTOR('',#8054,0.165);
#2339=VECTOR('',#8063,0.165);
#2340=VECTOR('',#8072,0.165);
#2341=VECTOR('',#8081,0.165);
#2342=VECTOR('',#8088,0.165);
#2343=VECTOR('',#8095,0.165);
#2344=VECTOR('',#8102,0.165);
#2345=VECTOR('',#8109,0.275);
#2346=VECTOR('',#8116,0.275);
#2347=VECTOR('',#8123,0.275);
#2348=VECTOR('',#8130,0.275);
#2349=VECTOR('',#8137,1.05);
#2350=VECTOR('',#8148,0.625);
#2351=VECTOR('',#8153,1.5);
#2352=VECTOR('',#8158,1.);
#2353=VECTOR('',#8161,1.);
#2354=VECTOR('',#8166,1.);
#2355=VECTOR('',#8167,1.);
#2356=VECTOR('',#8168,1.);
#2357=VECTOR('',#8169,1.);
#2358=VECTOR('',#8170,1.);
#2359=VECTOR('',#8171,1.);
#2360=VECTOR('',#8172,1.);
#2361=VECTOR('',#8175,1.);
#2362=VECTOR('',#8178,1.);
#2363=VECTOR('',#8179,1.);
#2364=VECTOR('',#8182,1.);
#2365=VECTOR('',#8183,1.);
#2366=VECTOR('',#8184,1.);
#2367=VECTOR('',#8185,1.);
#2368=VECTOR('',#8186,1.);
#2369=VECTOR('',#8187,1.);
#2370=VECTOR('',#8188,1.);
#2371=VECTOR('',#8191,1.);
#2372=VECTOR('',#8192,1.);
#2373=VECTOR('',#8193,1.);
#2374=VECTOR('',#8196,1.);
#2375=VECTOR('',#8197,1.);
#2376=VECTOR('',#8200,1.);
#2377=VECTOR('',#8201,1.);
#2378=VECTOR('',#8204,1.);
#2379=VECTOR('',#8207,1.);
#2380=VECTOR('',#8208,1.);
#2381=VECTOR('',#8211,1.);
#2382=VECTOR('',#8212,1.);
#2383=VECTOR('',#8217,1.);
#2384=VECTOR('',#8218,1.);
#2385=VECTOR('',#8219,1.);
#2386=VECTOR('',#8220,1.);
#2387=VECTOR('',#8221,1.);
#2388=VECTOR('',#8228,1.);
#2389=VECTOR('',#8231,1.);
#2390=VECTOR('',#8242,0.225);
#2391=VECTOR('',#8249,0.225);
#2392=VECTOR('',#8256,0.225);
#2393=VECTOR('',#8263,0.225);
#2394=VECTOR('',#8270,1.49);
#2395=VECTOR('',#8279,0.71);
#2396=VECTOR('',#8286,2.2);
#2397=VECTOR('',#8299,0.225);
#2398=VECTOR('',#8306,0.225);
#2399=VECTOR('',#8313,0.225);
#2400=VECTOR('',#8320,0.225);
#2401=VECTOR('',#8327,1.49);
#2402=VECTOR('',#8338,0.71);
#2403=VECTOR('',#8343,2.2);
#2404=VECTOR('',#8356,0.375);
#2405=VECTOR('',#8367,0.375);
#2406=VECTOR('',#8378,0.375);
#2407=VECTOR('',#8389,0.375);
#2408=VECTOR('',#8400,0.225);
#2409=VECTOR('',#8405,0.225);
#2410=VECTOR('',#8410,0.225);
#2411=VECTOR('',#8415,0.225);
#2412=VECTOR('',#8420,1.04);
#2413=VECTOR('',#8431,0.625);
#2414=VECTOR('',#8436,2.);
#2415=VECTOR('',#8447,1.);
#2416=VECTOR('',#8448,1.);
#2417=VECTOR('',#8449,1.);
#2418=VECTOR('',#8450,1.);
#2419=VECTOR('',#8453,1.);
#2420=VECTOR('',#8454,1.);
#2421=VECTOR('',#8455,1.);
#2422=VECTOR('',#8458,1.);
#2423=VECTOR('',#8459,1.);
#2424=VECTOR('',#8460,1.);
#2425=VECTOR('',#8463,1.);
#2426=VECTOR('',#8464,1.);
#2427=VECTOR('',#8475,0.165);
#2428=VECTOR('',#8484,0.165);
#2429=VECTOR('',#8491,1.);
#2430=VECTOR('',#8492,1.);
#2431=VECTOR('',#8493,1.);
#2432=VECTOR('',#8494,1.);
#2433=VECTOR('',#8497,1.);
#2434=VECTOR('',#8498,1.);
#2435=VECTOR('',#8499,1.);
#2436=VECTOR('',#8502,1.);
#2437=VECTOR('',#8503,1.);
#2438=VECTOR('',#8504,1.);
#2439=VECTOR('',#8507,1.);
#2440=VECTOR('',#8508,1.);
#2441=VECTOR('',#8519,0.165);
#2442=VECTOR('',#8528,0.165);
#2443=VECTOR('',#8535,1.);
#2444=VECTOR('',#8536,1.);
#2445=VECTOR('',#8537,1.);
#2446=VECTOR('',#8538,1.);
#2447=VECTOR('',#8541,1.);
#2448=VECTOR('',#8542,1.);
#2449=VECTOR('',#8543,1.);
#2450=VECTOR('',#8546,1.);
#2451=VECTOR('',#8547,1.);
#2452=VECTOR('',#8548,1.);
#2453=VECTOR('',#8551,1.);
#2454=VECTOR('',#8552,1.);
#2455=VECTOR('',#8563,0.165);
#2456=VECTOR('',#8578,0.5);
#2457=VECTOR('',#8583,0.3);
#2458=VECTOR('',#8592,1.);
#2459=VECTOR('',#8593,1.);
#2460=VECTOR('',#8594,1.);
#2461=VECTOR('',#8595,1.);
#2462=VECTOR('',#8598,1.);
#2463=VECTOR('',#8599,1.);
#2464=VECTOR('',#8600,1.);
#2465=VECTOR('',#8603,1.);
#2466=VECTOR('',#8604,1.);
#2467=VECTOR('',#8605,1.);
#2468=VECTOR('',#8608,1.);
#2469=VECTOR('',#8609,1.);
#2470=VECTOR('',#8610,1.);
#2471=VECTOR('',#8613,1.);
#2472=VECTOR('',#8614,1.);
#2473=VECTOR('',#8615,1.);
#2474=VECTOR('',#8618,1.);
#2475=VECTOR('',#8619,1.);
#2476=VECTOR('',#8636,0.4);
#2477=VECTOR('',#8641,0.425);
#2478=VECTOR('',#8646,0.41);
#2479=VECTOR('',#8655,0.26);
#2480=VECTOR('',#8658,0.25);
#2481=VECTOR('',#8677,0.976185);
#2482=VECTOR('',#8684,0.5);
#2483=VECTOR('',#8689,0.53);
#2484=VECTOR('',#8698,0.976185);
#2485=VECTOR('',#8705,0.53);
#2486=VECTOR('',#8724,1.023815);
#2487=VECTOR('',#8735,1.47);
#2488=VECTOR('',#8740,1.5);
#2489=VECTOR('',#8745,1.47);
#2490=VECTOR('',#8750,1.023815);
#2491=VECTOR('',#8801,1.019052);
#2492=VECTOR('',#8878,0.980948);
#2493=VECTOR('',#8907,1.013815);
#2494=VECTOR('',#8914,0.991185);
#2495=VECTOR('',#8925,1.013815);
#2496=VECTOR('',#8932,0.991185);
#2497=VECTOR('',#8951,1.);
#2498=VECTOR('',#8952,1.);
#2499=VECTOR('',#8953,1.);
#2500=VECTOR('',#8956,1.);
#2501=VECTOR('',#8957,1.);
#2502=VECTOR('',#8958,1.);
#2503=VECTOR('',#8963,1.);
#2504=VECTOR('',#8964,1.);
#2505=VECTOR('',#8967,1.);
#2506=VECTOR('',#8968,1.);
#2507=VECTOR('',#8981,1.05);
#2508=VECTOR('',#8990,1.);
#2509=VECTOR('',#8999,1.05);
#2510=VECTOR('',#9008,1.);
#2511=VECTOR('',#9017,1.05);
#2512=VECTOR('',#9024,0.9);
#2513=VECTOR('',#9031,1.);
#2514=VECTOR('',#9034,1.);
#2515=VECTOR('',#9037,1.);
#2516=VECTOR('',#9038,1.);
#2517=VECTOR('',#9039,1.);
#2518=VECTOR('',#9046,1.);
#2519=VECTOR('',#9049,1.);
#2520=VECTOR('',#9050,1.);
#2521=VECTOR('',#9061,0.895);
#2522=VECTOR('',#9068,0.605);
#2523=VECTOR('',#9077,1.);
#2524=VECTOR('',#9078,1.);
#2525=VECTOR('',#9079,1.);
#2526=VECTOR('',#9080,1.);
#2527=VECTOR('',#9083,1.);
#2528=VECTOR('',#9084,1.);
#2529=VECTOR('',#9085,1.);
#2530=VECTOR('',#9088,1.);
#2531=VECTOR('',#9089,1.);
#2532=VECTOR('',#9090,1.);
#2533=VECTOR('',#9093,1.);
#2534=VECTOR('',#9094,1.);
#2535=VECTOR('',#9095,1.);
#2536=VECTOR('',#9098,1.);
#2537=VECTOR('',#9099,1.);
#2538=VECTOR('',#9100,1.);
#2539=VECTOR('',#9103,1.);
#2540=VECTOR('',#9104,1.);
#2541=VECTOR('',#9117,0.2);
#2542=VECTOR('',#9130,0.325);
#2543=VECTOR('',#9135,0.35);
#2544=VECTOR('',#9140,0.335);
#2545=VECTOR('',#9149,0.21);
#2546=VECTOR('',#9154,0.2);
#2547=VECTOR('',#9157,0.18);
#2548=VECTOR('',#9166,0.305);
#2549=VECTOR('',#9171,1.);
#2550=VECTOR('',#9174,1.);
#2551=VECTOR('',#9179,1.);
#2552=VECTOR('',#9184,1.);
#2553=VECTOR('',#9187,1.);
#2554=VECTOR('',#9190,1.);
#2555=VECTOR('',#9195,1.);
#2556=VECTOR('',#9196,1.);
#2557=VECTOR('',#9199,1.);
#2558=VECTOR('',#9204,1.);
#2559=VECTOR('',#9207,1.);
#2560=VECTOR('',#9210,1.);
#2561=VECTOR('',#9213,1.);
#2562=VECTOR('',#9214,1.);
#2563=VECTOR('',#9217,1.);
#2564=VECTOR('',#9222,1.);
#2565=VECTOR('',#9231,1.);
#2566=VECTOR('',#9240,0.7);
#2567=VECTOR('',#9243,0.5);
#2568=VECTOR('',#9250,0.5);
#2569=VECTOR('',#9261,0.505);
#2570=VECTOR('',#9268,0.7);
#2571=VECTOR('',#9279,1.);
#2572=VECTOR('',#9286,0.164999999999999);
#2573=VECTOR('',#9291,1.);
#2574=VECTOR('',#9296,0.505);
#2575=VECTOR('',#9303,0.9);
#2576=VECTOR('',#9316,0.165);
#2577=VECTOR('',#9325,0.165);
#2578=VECTOR('',#9344,0.7);
#2579=VECTOR('',#9347,0.3);
#2580=VECTOR('',#9354,0.3);
#2581=VECTOR('',#9365,0.305);
#2582=VECTOR('',#9372,0.5);
#2583=VECTOR('',#9385,0.305);
#2584=VECTOR('',#9392,0.5);
#2585=VECTOR('',#9405,0.225);
#2586=VECTOR('',#9412,0.5);
#2587=VECTOR('',#9425,0.225);
#2588=VECTOR('',#9432,0.5);
#2589=VECTOR('',#9447,1.);
#2590=VECTOR('',#9448,1.);
#2591=VECTOR('',#9449,1.);
#2592=VECTOR('',#9450,1.);
#2593=VECTOR('',#9453,1.);
#2594=VECTOR('',#9454,1.);
#2595=VECTOR('',#9455,1.);
#2596=VECTOR('',#9458,1.);
#2597=VECTOR('',#9459,1.);
#2598=VECTOR('',#9460,1.);
#2599=VECTOR('',#9463,1.);
#2600=VECTOR('',#9464,1.);
#2601=VECTOR('',#9465,1.);
#2602=VECTOR('',#9468,1.);
#2603=VECTOR('',#9469,1.);
#2604=VECTOR('',#9470,1.);
#2605=VECTOR('',#9473,1.);
#2606=VECTOR('',#9474,1.);
#2607=VECTOR('',#9485,0.185);
#2608=VECTOR('',#9488,0.2);
#2609=VECTOR('',#9493,1.);
#2610=VECTOR('',#9494,1.);
#2611=VECTOR('',#9495,1.);
#2612=VECTOR('',#9496,1.);
#2613=VECTOR('',#9499,1.);
#2614=VECTOR('',#9500,1.);
#2615=VECTOR('',#9501,1.);
#2616=VECTOR('',#9504,1.);
#2617=VECTOR('',#9505,1.);
#2618=VECTOR('',#9506,1.);
#2619=VECTOR('',#9509,1.);
#2620=VECTOR('',#9510,1.);
#2621=VECTOR('',#9511,1.);
#2622=VECTOR('',#9514,1.);
#2623=VECTOR('',#9515,1.);
#2624=VECTOR('',#9516,1.);
#2625=VECTOR('',#9519,1.);
#2626=VECTOR('',#9520,1.);
#2627=VECTOR('',#9537,0.325);
#2628=VECTOR('',#9542,0.35);
#2629=VECTOR('',#9547,0.335);
#2630=VECTOR('',#9556,0.21);
#2631=VECTOR('',#9559,0.2);
#2632=VECTOR('',#9570,0.325);
#2633=VECTOR('',#9575,0.35);
#2634=VECTOR('',#9580,0.335);
#2635=VECTOR('',#9589,0.21);
#2636=VECTOR('',#9594,0.2);
#2637=VECTOR('',#9599,0.18);
#2638=VECTOR('',#9604,1.);
#2639=VECTOR('',#9605,1.);
#2640=VECTOR('',#9606,1.);
#2641=VECTOR('',#9607,1.);
#2642=VECTOR('',#9610,1.);
#2643=VECTOR('',#9611,1.);
#2644=VECTOR('',#9612,1.);
#2645=VECTOR('',#9615,1.);
#2646=VECTOR('',#9616,1.);
#2647=VECTOR('',#9617,1.);
#2648=VECTOR('',#9620,1.);
#2649=VECTOR('',#9621,1.);
#2650=VECTOR('',#9622,1.);
#2651=VECTOR('',#9625,1.);
#2652=VECTOR('',#9626,1.);
#2653=VECTOR('',#9627,1.);
#2654=VECTOR('',#9630,1.);
#2655=VECTOR('',#9631,1.);
#2656=VECTOR('',#9734,0.5);
#2657=VECTOR('',#9741,0.5);
#2658=VECTOR('',#9746,1.);
#2659=VECTOR('',#9749,1.);
#2660=VECTOR('',#9754,1.);
#2661=VECTOR('',#9755,1.);
#2662=VECTOR('',#9756,1.);
#2663=VECTOR('',#9759,1.);
#2664=VECTOR('',#9764,1.);
#2665=VECTOR('',#9765,1.);
#2666=VECTOR('',#9778,0.305);
#2667=VECTOR('',#9785,0.5);
#2668=VECTOR('',#9798,0.305);
#2669=VECTOR('',#9805,0.5);
#2670=VECTOR('',#9826,0.305);
#2671=VECTOR('',#9833,1.);
#2672=VECTOR('',#9834,1.);
#2673=VECTOR('',#9835,1.);
#2674=VECTOR('',#9836,1.);
#2675=VECTOR('',#9839,1.);
#2676=VECTOR('',#9840,1.);
#2677=VECTOR('',#9841,1.);
#2678=VECTOR('',#9842,1.);
#2679=VECTOR('',#9843,1.);
#2680=VECTOR('',#9846,1.);
#2681=VECTOR('',#9851,1.);
#2682=VECTOR('',#9852,1.);
#2683=VECTOR('',#9853,1.);
#2684=VECTOR('',#9854,1.);
#2685=VECTOR('',#9857,1.);
#2686=VECTOR('',#9858,1.);
#2687=VECTOR('',#9859,1.);
#2688=VECTOR('',#9862,1.);
#2689=VECTOR('',#9863,1.);
#2690=VECTOR('',#9864,1.);
#2691=VECTOR('',#9873,0.6);
#2692=VECTOR('',#9884,1.2);
#2693=VECTOR('',#9893,1.);
#2694=VECTOR('',#9900,0.165);
#2695=VECTOR('',#9907,1.);
#2696=VECTOR('',#9912,0.305);
#2697=VECTOR('',#9917,1.);
#2698=VECTOR('',#9918,1.);
#2699=VECTOR('',#9919,1.);
#2700=VECTOR('',#9920,1.);
#2701=VECTOR('',#9923,1.);
#2702=VECTOR('',#9924,1.);
#2703=VECTOR('',#9925,1.);
#2704=VECTOR('',#9928,1.);
#2705=VECTOR('',#9929,1.);
#2706=VECTOR('',#9932,1.);
#2707=VECTOR('',#9933,1.);
#2708=VECTOR('',#9936,1.);
#2709=VECTOR('',#9949,0.5);
#2710=VECTOR('',#9958,0.3);
#2711=VECTOR('',#9967,1.);
#2712=VECTOR('',#9978,1.);
#2713=VECTOR('',#9979,1.);
#2714=VECTOR('',#9980,1.);
#2715=VECTOR('',#9981,1.);
#2716=VECTOR('',#9984,1.);
#2717=VECTOR('',#9985,1.);
#2718=VECTOR('',#9986,1.);
#2719=VECTOR('',#9989,1.);
#2720=VECTOR('',#9990,1.);
#2721=VECTOR('',#9991,1.);
#2722=VECTOR('',#9994,1.);
#2723=VECTOR('',#9995,1.);
#2724=VECTOR('',#9996,1.);
#2725=VECTOR('',#9999,1.);
#2726=VECTOR('',#10000,1.);
#2727=VECTOR('',#10001,1.);
#2728=VECTOR('',#10004,1.);
#2729=VECTOR('',#10005,1.);
#2730=VECTOR('',#10016,0.185);
#2731=VECTOR('',#10021,0.2);
#2732=VECTOR('',#10026,0.1625);
#2733=CIRCLE('',#7043,0.225);
#2734=CIRCLE('',#7044,0.225);
#2735=CIRCLE('',#7046,0.225);
#2736=CIRCLE('',#7047,0.225);
#2737=CIRCLE('',#7049,0.225);
#2738=CIRCLE('',#7050,0.225);
#2739=CIRCLE('',#7052,0.225);
#2740=CIRCLE('',#7053,0.225);
#2741=CIRCLE('',#7055,0.21);
#2742=CIRCLE('',#7056,0.21);
#2743=CIRCLE('',#7058,0.210000000000001);
#2744=CIRCLE('',#7059,0.210000000000001);
#2745=CIRCLE('',#7061,0.210000000000001);
#2746=CIRCLE('',#7062,0.210000000000001);
#2747=CIRCLE('',#7064,0.21);
#2748=CIRCLE('',#7065,0.21);
#2749=CIRCLE('',#7088,0.225);
#2750=CIRCLE('',#7089,0.225);
#2751=CIRCLE('',#7091,0.165);
#2752=CIRCLE('',#7092,0.165);
#2753=CIRCLE('',#7095,0.165);
#2754=CIRCLE('',#7096,0.165);
#2755=CIRCLE('',#7099,0.165);
#2756=CIRCLE('',#7100,0.165);
#2757=CIRCLE('',#7103,0.165);
#2758=CIRCLE('',#7104,0.165);
#2759=CIRCLE('',#7107,0.165);
#2760=CIRCLE('',#7108,0.165);
#2761=CIRCLE('',#7110,0.165);
#2762=CIRCLE('',#7111,0.165);
#2763=CIRCLE('',#7113,0.165);
#2764=CIRCLE('',#7114,0.165);
#2765=CIRCLE('',#7116,0.165);
#2766=CIRCLE('',#7117,0.165);
#2767=CIRCLE('',#7119,0.275);
#2768=CIRCLE('',#7120,0.275);
#2769=CIRCLE('',#7122,0.275);
#2770=CIRCLE('',#7123,0.275);
#2771=CIRCLE('',#7125,0.275);
#2772=CIRCLE('',#7126,0.275);
#2773=CIRCLE('',#7128,0.275);
#2774=CIRCLE('',#7129,0.275);
#2775=CIRCLE('',#7131,1.05);
#2776=CIRCLE('',#7132,1.05);
#2777=CIRCLE('',#7134,0.625);
#2778=CIRCLE('',#7136,0.625);
#2779=CIRCLE('',#7138,1.5);
#2780=CIRCLE('',#7139,1.5);
#2781=CIRCLE('',#7141,2.);
#2782=CIRCLE('',#7142,2.);
#2783=CIRCLE('',#7144,2.2);
#2784=CIRCLE('',#7153,2.2);
#2785=CIRCLE('',#7163,0.225);
#2786=CIRCLE('',#7164,0.225);
#2787=CIRCLE('',#7166,0.225);
#2788=CIRCLE('',#7167,0.225);
#2789=CIRCLE('',#7169,0.225);
#2790=CIRCLE('',#7170,0.225);
#2791=CIRCLE('',#7172,0.225);
#2792=CIRCLE('',#7173,0.225);
#2793=CIRCLE('',#7175,1.49);
#2794=CIRCLE('',#7176,1.49);
#2795=CIRCLE('',#7178,0.71);
#2796=CIRCLE('',#7180,0.71);
#2797=CIRCLE('',#7182,2.2);
#2798=CIRCLE('',#7183,2.2);
#2799=CIRCLE('',#7188,0.225);
#2800=CIRCLE('',#7189,0.225);
#2801=CIRCLE('',#7191,0.225);
#2802=CIRCLE('',#7192,0.225);
#2803=CIRCLE('',#7194,0.225);
#2804=CIRCLE('',#7195,0.225);
#2805=CIRCLE('',#7197,0.225);
#2806=CIRCLE('',#7198,0.225);
#2807=CIRCLE('',#7200,1.49);
#2808=CIRCLE('',#7201,1.49);
#2809=CIRCLE('',#7203,0.71);
#2810=CIRCLE('',#7205,0.71);
#2811=CIRCLE('',#7207,2.2);
#2812=CIRCLE('',#7208,2.2);
#2813=CIRCLE('',#7213,0.375);
#2814=CIRCLE('',#7214,0.375);
#2815=CIRCLE('',#7216,0.225);
#2816=CIRCLE('',#7218,0.375);
#2817=CIRCLE('',#7219,0.375);
#2818=CIRCLE('',#7221,0.225);
#2819=CIRCLE('',#7223,0.375);
#2820=CIRCLE('',#7224,0.375);
#2821=CIRCLE('',#7226,0.225);
#2822=CIRCLE('',#7228,0.375);
#2823=CIRCLE('',#7229,0.375);
#2824=CIRCLE('',#7231,0.225);
#2825=CIRCLE('',#7233,0.225);
#2826=CIRCLE('',#7235,0.225);
#2827=CIRCLE('',#7237,0.225);
#2828=CIRCLE('',#7239,0.225);
#2829=CIRCLE('',#7241,1.04);
#2830=CIRCLE('',#7242,1.04);
#2831=CIRCLE('',#7244,0.625);
#2832=CIRCLE('',#7246,0.625);
#2833=CIRCLE('',#7248,2.);
#2834=CIRCLE('',#7249,2.);
#2835=CIRCLE('',#7261,0.165);
#2836=CIRCLE('',#7262,0.165);
#2837=CIRCLE('',#7265,0.165);
#2838=CIRCLE('',#7266,0.165);
#2839=CIRCLE('',#7276,0.165);
#2840=CIRCLE('',#7277,0.165);
#2841=CIRCLE('',#7280,0.165);
#2842=CIRCLE('',#7281,0.165);
#2843=CIRCLE('',#7291,0.165);
#2844=CIRCLE('',#7292,0.165);
#2845=CIRCLE('',#7295,0.5);
#2846=CIRCLE('',#7296,0.3);
#2847=CIRCLE('',#7298,0.5);
#2848=CIRCLE('',#7301,0.3);
#2849=CIRCLE('',#7313,0.24505);
#2850=CIRCLE('',#7315,0.375);
#2851=CIRCLE('',#7317,0.425);
#2852=CIRCLE('',#7319,0.425);
#2853=CIRCLE('',#7321,0.395);
#2854=CIRCLE('',#7323,0.27);
#2855=CIRCLE('',#7325,0.24505);
#2856=CIRCLE('',#7330,0.976185);
#2857=CIRCLE('',#7331,0.976185);
#2858=CIRCLE('',#7332,0.247676);
#2859=CIRCLE('',#7333,0.976185);
#2860=CIRCLE('',#7334,0.976185);
#2861=CIRCLE('',#7336,0.976185);
#2862=CIRCLE('',#7338,0.5);
#2863=CIRCLE('',#7339,0.5);
#2864=CIRCLE('',#7341,0.56);
#2865=CIRCLE('',#7344,0.976185);
#2866=CIRCLE('',#7346,0.56);
#2867=CIRCLE('',#7350,1.023815);
#2868=CIRCLE('',#7351,1.023815);
#2869=CIRCLE('',#7352,0.247676);
#2870=CIRCLE('',#7353,1.023815);
#2871=CIRCLE('',#7354,1.023815);
#2872=CIRCLE('',#7356,1.023815);
#2873=CIRCLE('',#7358,1.44);
#2874=CIRCLE('',#7359,1.023815);
#2875=CIRCLE('',#7361,1.5);
#2876=CIRCLE('',#7363,1.5);
#2877=CIRCLE('',#7365,1.44);
#2878=CIRCLE('',#7370,0.23815);
#2879=CIRCLE('',#7372,0.23815);
#2880=CIRCLE('',#7374,0.23815);
#2881=CIRCLE('',#7376,0.23815);
#2882=CIRCLE('',#7378,0.23815);
#2883=CIRCLE('',#7380,0.23815);
#2884=CIRCLE('',#7382,0.23815);
#2885=CIRCLE('',#7384,0.23815);
#2886=CIRCLE('',#7387,0.243053047864041);
#2887=CIRCLE('',#7388,0.243053047864041);
#2888=CIRCLE('',#7390,1.019052);
#2889=CIRCLE('',#7391,1.019052);
#2890=CIRCLE('',#7392,1.019052);
#2891=CIRCLE('',#7393,1.019052);
#2892=CIRCLE('',#7394,1.019052);
#2893=CIRCLE('',#7395,1.019052);
#2894=CIRCLE('',#7396,1.019052);
#2895=CIRCLE('',#7397,1.019052);
#2896=CIRCLE('',#7398,1.019052);
#2897=CIRCLE('',#7400,0.980948);
#2898=CIRCLE('',#7401,0.243053047864041);
#2899=CIRCLE('',#7403,0.243053047864041);
#2900=CIRCLE('',#7405,0.980948);
#2901=CIRCLE('',#7406,0.243053047864041);
#2902=CIRCLE('',#7408,0.243053047864041);
#2903=CIRCLE('',#7410,0.980948);
#2904=CIRCLE('',#7411,0.243053047864041);
#2905=CIRCLE('',#7413,0.243053047864041);
#2906=CIRCLE('',#7415,0.980948);
#2907=CIRCLE('',#7416,0.243053047864041);
#2908=CIRCLE('',#7418,0.243053047864041);
#2909=CIRCLE('',#7420,0.980948);
#2910=CIRCLE('',#7421,0.243053047864041);
#2911=CIRCLE('',#7423,0.243053047864041);
#2912=CIRCLE('',#7425,0.980948);
#2913=CIRCLE('',#7426,0.243053047864041);
#2914=CIRCLE('',#7428,0.243053047864041);
#2915=CIRCLE('',#7430,0.980948);
#2916=CIRCLE('',#7431,0.980948);
#2917=CIRCLE('',#7432,0.980948);
#2918=CIRCLE('',#7434,0.243053047864041);
#2919=CIRCLE('',#7436,0.243053047864041);
#2920=CIRCLE('',#7441,1.013815);
#2921=CIRCLE('',#7442,0.991185);
#2922=CIRCLE('',#7444,1.013815);
#2923=CIRCLE('',#7446,0.991185);
#2924=CIRCLE('',#7449,1.013815);
#2925=CIRCLE('',#7450,0.991185);
#2926=CIRCLE('',#7452,1.013815);
#2927=CIRCLE('',#7454,0.991185);
#2928=CIRCLE('',#7464,0.9);
#2929=CIRCLE('',#7467,0.9);
#2930=CIRCLE('',#7471,1.05);
#2931=CIRCLE('',#7472,0.9);
#2932=CIRCLE('',#7474,1.05);
#2933=CIRCLE('',#7476,1.);
#2934=CIRCLE('',#7478,1.);
#2935=CIRCLE('',#7480,1.05);
#2936=CIRCLE('',#7482,1.05);
#2937=CIRCLE('',#7484,1.);
#2938=CIRCLE('',#7486,1.);
#2939=CIRCLE('',#7488,1.05);
#2940=CIRCLE('',#7490,1.05);
#2941=CIRCLE('',#7492,0.9);
#2942=CIRCLE('',#7496,0.895);
#2943=CIRCLE('',#7497,0.605);
#2944=CIRCLE('',#7500,0.895);
#2945=CIRCLE('',#7501,0.605);
#2946=CIRCLE('',#7504,0.895);
#2947=CIRCLE('',#7505,0.605);
#2948=CIRCLE('',#7507,0.895);
#2949=CIRCLE('',#7509,0.605);
#2950=CIRCLE('',#7523,0.2);
#2951=CIRCLE('',#7524,0.16);
#2952=CIRCLE('',#7526,0.2);
#2953=CIRCLE('',#7529,0.3);
#2954=CIRCLE('',#7531,0.35);
#2955=CIRCLE('',#7533,0.35);
#2956=CIRCLE('',#7535,0.32);
#2957=CIRCLE('',#7537,0.22);
#2958=CIRCLE('',#7539,0.1954);
#2959=CIRCLE('',#7541,0.1954);
#2960=CIRCLE('',#7546,0.305);
#2961=CIRCLE('',#7547,0.305);
#2962=CIRCLE('',#7549,0.8);
#2963=CIRCLE('',#7550,0.8);
#2964=CIRCLE('',#7552,1.);
#2965=CIRCLE('',#7553,1.);
#2966=CIRCLE('',#7554,0.7);
#2967=CIRCLE('',#7555,1.);
#2968=CIRCLE('',#7556,0.5);
#2969=CIRCLE('',#7559,1.);
#2970=CIRCLE('',#7562,0.7);
#2971=CIRCLE('',#7565,1.);
#2972=CIRCLE('',#7568,1.);
#2973=CIRCLE('',#7569,0.7);
#2974=CIRCLE('',#7572,0.7);
#2975=CIRCLE('',#7573,0.5);
#2976=CIRCLE('',#7576,0.5);
#2977=CIRCLE('',#7578,0.5);
#2978=CIRCLE('',#7583,0.505);
#2979=CIRCLE('',#7584,0.505);
#2980=CIRCLE('',#7586,0.7);
#2981=CIRCLE('',#7587,0.7);
#2982=CIRCLE('',#7592,0.164999999999999);
#2983=CIRCLE('',#7594,0.164999999999999);
#2984=CIRCLE('',#7595,0.164999999999999);
#2985=CIRCLE('',#7598,0.505);
#2986=CIRCLE('',#7599,0.505);
#2987=CIRCLE('',#7601,0.9);
#2988=CIRCLE('',#7602,0.9);
#2989=CIRCLE('',#7607,0.165);
#2990=CIRCLE('',#7608,0.165);
#2991=CIRCLE('',#7611,0.165);
#2992=CIRCLE('',#7612,0.165);
#2993=CIRCLE('',#7615,0.7);
#2994=CIRCLE('',#7616,0.3);
#2995=CIRCLE('',#7618,0.7);
#2996=CIRCLE('',#7619,0.3);
#2997=CIRCLE('',#7622,0.3);
#2998=CIRCLE('',#7624,0.3);
#2999=CIRCLE('',#7629,0.305);
#3000=CIRCLE('',#7630,0.305);
#3001=CIRCLE('',#7632,0.5);
#3002=CIRCLE('',#7633,0.5);
#3003=CIRCLE('',#7638,0.305);
#3004=CIRCLE('',#7639,0.305);
#3005=CIRCLE('',#7641,0.5);
#3006=CIRCLE('',#7642,0.5);
#3007=CIRCLE('',#7647,0.225);
#3008=CIRCLE('',#7648,0.225);
#3009=CIRCLE('',#7650,0.5);
#3010=CIRCLE('',#7651,0.5);
#3011=CIRCLE('',#7656,0.225);
#3012=CIRCLE('',#7657,0.225);
#3013=CIRCLE('',#7659,0.5);
#3014=CIRCLE('',#7660,0.5);
#3015=CIRCLE('',#7665,0.1954);
#3016=CIRCLE('',#7674,0.17);
#3017=CIRCLE('',#7676,0.1954);
#3018=CIRCLE('',#7688,0.1954);
#3019=CIRCLE('',#7690,0.3);
#3020=CIRCLE('',#7692,0.35);
#3021=CIRCLE('',#7694,0.35);
#3022=CIRCLE('',#7696,0.32);
#3023=CIRCLE('',#7698,0.22);
#3024=CIRCLE('',#7700,0.1954);
#3025=CIRCLE('',#7704,0.3);
#3026=CIRCLE('',#7706,0.35);
#3027=CIRCLE('',#7708,0.35);
#3028=CIRCLE('',#7710,0.32);
#3029=CIRCLE('',#7712,0.22);
#3030=CIRCLE('',#7714,0.1954);
#3031=CIRCLE('',#7716,0.1954);
#3032=CIRCLE('',#7718,0.16);
#3033=CIRCLE('',#7776,0.5);
#3034=CIRCLE('',#7777,0.5);
#3035=CIRCLE('',#7779,0.5);
#3036=CIRCLE('',#7780,0.5);
#3037=CIRCLE('',#7782,0.8);
#3038=CIRCLE('',#7783,0.8);
#3039=CIRCLE('',#7786,0.8);
#3040=CIRCLE('',#7789,0.8);
#3041=CIRCLE('',#7793,0.305);
#3042=CIRCLE('',#7794,0.305);
#3043=CIRCLE('',#7796,0.5);
#3044=CIRCLE('',#7797,0.5);
#3045=CIRCLE('',#7802,0.305);
#3046=CIRCLE('',#7803,0.305);
#3047=CIRCLE('',#7805,0.5);
#3048=CIRCLE('',#7806,0.5);
#3049=CIRCLE('',#7815,0.305);
#3050=CIRCLE('',#7816,0.305);
#3051=CIRCLE('',#7821,1.2);
#3052=CIRCLE('',#7826,0.6);
#3053=CIRCLE('',#7828,0.6);
#3054=CIRCLE('',#7829,0.6);
#3055=CIRCLE('',#7831,1.2);
#3056=CIRCLE('',#7832,1.2);
#3057=CIRCLE('',#7834,1.2);
#3058=CIRCLE('',#7838,0.165);
#3059=CIRCLE('',#7840,0.165);
#3060=CIRCLE('',#7841,0.165);
#3061=CIRCLE('',#7842,0.165);
#3062=CIRCLE('',#7845,0.305);
#3063=CIRCLE('',#7846,0.305);
#3064=CIRCLE('',#7855,0.5);
#3065=CIRCLE('',#7856,0.3);
#3066=CIRCLE('',#7858,0.5);
#3067=CIRCLE('',#7861,0.3);
#3068=CIRCLE('',#7865,1.);
#3069=CIRCLE('',#7866,1.);
#3070=CIRCLE('',#7878,0.17);
#3071=CIRCLE('',#7880,0.1954);
#3072=CIRCLE('',#7882,0.1954);
#3073=CIRCLE('',#7884,0.125);
#3074=VERTEX_POINT('',#10049);
#3075=VERTEX_POINT('',#10051);
#3076=VERTEX_POINT('',#10055);
#3077=VERTEX_POINT('',#10057);
#3078=VERTEX_POINT('',#10061);
#3079=VERTEX_POINT('',#10063);
#3080=VERTEX_POINT('',#10067);
#3081=VERTEX_POINT('',#10069);
#3082=VERTEX_POINT('',#10073);
#3083=VERTEX_POINT('',#10075);
#3084=VERTEX_POINT('',#10079);
#3085=VERTEX_POINT('',#10081);
#3086=VERTEX_POINT('',#10085);
#3087=VERTEX_POINT('',#10087);
#3088=VERTEX_POINT('',#10091);
#3089=VERTEX_POINT('',#10093);
#3090=VERTEX_POINT('',#10097);
#3091=VERTEX_POINT('',#10098);
#3092=VERTEX_POINT('',#10100);
#3093=VERTEX_POINT('',#10102);
#3094=VERTEX_POINT('',#10106);
#3095=VERTEX_POINT('',#10108);
#3096=VERTEX_POINT('',#10112);
#3097=VERTEX_POINT('',#10114);
#3098=VERTEX_POINT('',#10124);
#3099=VERTEX_POINT('',#10125);
#3100=VERTEX_POINT('',#10127);
#3101=VERTEX_POINT('',#10129);
#3102=VERTEX_POINT('',#10133);
#3103=VERTEX_POINT('',#10135);
#3104=VERTEX_POINT('',#10139);
#3105=VERTEX_POINT('',#10141);
#3106=VERTEX_POINT('',#10151);
#3107=VERTEX_POINT('',#10152);
#3108=VERTEX_POINT('',#10154);
#3109=VERTEX_POINT('',#10156);
#3110=VERTEX_POINT('',#10160);
#3111=VERTEX_POINT('',#10162);
#3112=VERTEX_POINT('',#10166);
#3113=VERTEX_POINT('',#10168);
#3114=VERTEX_POINT('',#10178);
#3115=VERTEX_POINT('',#10180);
#3116=VERTEX_POINT('',#10184);
#3117=VERTEX_POINT('',#10186);
#3118=VERTEX_POINT('',#10191);
#3119=VERTEX_POINT('',#10193);
#3120=VERTEX_POINT('',#10198);
#3121=VERTEX_POINT('',#10200);
#3122=VERTEX_POINT('',#10205);
#3123=VERTEX_POINT('',#10207);
#3124=VERTEX_POINT('',#10212);
#3125=VERTEX_POINT('',#10214);
#3126=VERTEX_POINT('',#10218);
#3127=VERTEX_POINT('',#10220);
#3128=VERTEX_POINT('',#10224);
#3129=VERTEX_POINT('',#10226);
#3130=VERTEX_POINT('',#10230);
#3131=VERTEX_POINT('',#10232);
#3132=VERTEX_POINT('',#10236);
#3133=VERTEX_POINT('',#10238);
#3134=VERTEX_POINT('',#10242);
#3135=VERTEX_POINT('',#10244);
#3136=VERTEX_POINT('',#10248);
#3137=VERTEX_POINT('',#10250);
#3138=VERTEX_POINT('',#10254);
#3139=VERTEX_POINT('',#10256);
#3140=VERTEX_POINT('',#10260);
#3141=VERTEX_POINT('',#10262);
#3142=VERTEX_POINT('',#10266);
#3143=VERTEX_POINT('',#10269);
#3144=VERTEX_POINT('',#10273);
#3145=VERTEX_POINT('',#10275);
#3146=VERTEX_POINT('',#10279);
#3147=VERTEX_POINT('',#10280);
#3148=VERTEX_POINT('',#10282);
#3149=VERTEX_POINT('',#10284);
#3150=VERTEX_POINT('',#10288);
#3151=VERTEX_POINT('',#10290);
#3152=VERTEX_POINT('',#10292);
#3153=VERTEX_POINT('',#10294);
#3154=VERTEX_POINT('',#10296);
#3155=VERTEX_POINT('',#10298);
#3156=VERTEX_POINT('',#10300);
#3157=VERTEX_POINT('',#10302);
#3158=VERTEX_POINT('',#10306);
#3159=VERTEX_POINT('',#10310);
#3160=VERTEX_POINT('',#10311);
#3161=VERTEX_POINT('',#10313);
#3162=VERTEX_POINT('',#10315);
#3163=VERTEX_POINT('',#10318);
#3164=VERTEX_POINT('',#10319);
#3165=VERTEX_POINT('',#10324);
#3166=VERTEX_POINT('',#10325);
#3167=VERTEX_POINT('',#10330);
#3168=VERTEX_POINT('',#10334);
#3169=VERTEX_POINT('',#10340);
#3170=VERTEX_POINT('',#10344);
#3171=VERTEX_POINT('',#10346);
#3172=VERTEX_POINT('',#10352);
#3173=VERTEX_POINT('',#10354);
#3174=VERTEX_POINT('',#10367);
#3175=VERTEX_POINT('',#10369);
#3176=VERTEX_POINT('',#10373);
#3177=VERTEX_POINT('',#10375);
#3178=VERTEX_POINT('',#10379);
#3179=VERTEX_POINT('',#10381);
#3180=VERTEX_POINT('',#10385);
#3181=VERTEX_POINT('',#10387);
#3182=VERTEX_POINT('',#10391);
#3183=VERTEX_POINT('',#10393);
#3184=VERTEX_POINT('',#10397);
#3185=VERTEX_POINT('',#10400);
#3186=VERTEX_POINT('',#10404);
#3187=VERTEX_POINT('',#10406);
#3188=VERTEX_POINT('',#10413);
#3189=VERTEX_POINT('',#10415);
#3190=VERTEX_POINT('',#10419);
#3191=VERTEX_POINT('',#10421);
#3192=VERTEX_POINT('',#10425);
#3193=VERTEX_POINT('',#10427);
#3194=VERTEX_POINT('',#10431);
#3195=VERTEX_POINT('',#10433);
#3196=VERTEX_POINT('',#10437);
#3197=VERTEX_POINT('',#10439);
#3198=VERTEX_POINT('',#10443);
#3199=VERTEX_POINT('',#10446);
#3200=VERTEX_POINT('',#10450);
#3201=VERTEX_POINT('',#10452);
#3202=VERTEX_POINT('',#10459);
#3203=VERTEX_POINT('',#10461);
#3204=VERTEX_POINT('',#10465);
#3205=VERTEX_POINT('',#10468);
#3206=VERTEX_POINT('',#10470);
#3207=VERTEX_POINT('',#10474);
#3208=VERTEX_POINT('',#10477);
#3209=VERTEX_POINT('',#10479);
#3210=VERTEX_POINT('',#10483);
#3211=VERTEX_POINT('',#10486);
#3212=VERTEX_POINT('',#10488);
#3213=VERTEX_POINT('',#10492);
#3214=VERTEX_POINT('',#10495);
#3215=VERTEX_POINT('',#10499);
#3216=VERTEX_POINT('',#10503);
#3217=VERTEX_POINT('',#10507);
#3218=VERTEX_POINT('',#10511);
#3219=VERTEX_POINT('',#10513);
#3220=VERTEX_POINT('',#10517);
#3221=VERTEX_POINT('',#10520);
#3222=VERTEX_POINT('',#10524);
#3223=VERTEX_POINT('',#10526);
#3224=VERTEX_POINT('',#10533);
#3225=VERTEX_POINT('',#10534);
#3226=VERTEX_POINT('',#10536);
#3227=VERTEX_POINT('',#10538);
#3228=VERTEX_POINT('',#10542);
#3229=VERTEX_POINT('',#10544);
#3230=VERTEX_POINT('',#10548);
#3231=VERTEX_POINT('',#10550);
#3232=VERTEX_POINT('',#10560);
#3233=VERTEX_POINT('',#10562);
#3234=VERTEX_POINT('',#10567);
#3235=VERTEX_POINT('',#10569);
#3236=VERTEX_POINT('',#10574);
#3237=VERTEX_POINT('',#10575);
#3238=VERTEX_POINT('',#10577);
#3239=VERTEX_POINT('',#10579);
#3240=VERTEX_POINT('',#10583);
#3241=VERTEX_POINT('',#10585);
#3242=VERTEX_POINT('',#10589);
#3243=VERTEX_POINT('',#10591);
#3244=VERTEX_POINT('',#10601);
#3245=VERTEX_POINT('',#10603);
#3246=VERTEX_POINT('',#10608);
#3247=VERTEX_POINT('',#10610);
#3248=VERTEX_POINT('',#10615);
#3249=VERTEX_POINT('',#10616);
#3250=VERTEX_POINT('',#10618);
#3251=VERTEX_POINT('',#10620);
#3252=VERTEX_POINT('',#10624);
#3253=VERTEX_POINT('',#10626);
#3254=VERTEX_POINT('',#10630);
#3255=VERTEX_POINT('',#10632);
#3256=VERTEX_POINT('',#10642);
#3257=VERTEX_POINT('',#10644);
#3258=VERTEX_POINT('',#10649);
#3259=VERTEX_POINT('',#10651);
#3260=VERTEX_POINT('',#10654);
#3261=VERTEX_POINT('',#10659);
#3262=VERTEX_POINT('',#10665);
#3263=VERTEX_POINT('',#10666);
#3264=VERTEX_POINT('',#10668);
#3265=VERTEX_POINT('',#10670);
#3266=VERTEX_POINT('',#10674);
#3267=VERTEX_POINT('',#10676);
#3268=VERTEX_POINT('',#10680);
#3269=VERTEX_POINT('',#10682);
#3270=VERTEX_POINT('',#10686);
#3271=VERTEX_POINT('',#10688);
#3272=VERTEX_POINT('',#10692);
#3273=VERTEX_POINT('',#10694);
#3274=VERTEX_POINT('',#10703);
#3275=VERTEX_POINT('',#10706);
#3276=VERTEX_POINT('',#10709);
#3277=VERTEX_POINT('',#10713);
#3278=VERTEX_POINT('',#10717);
#3279=VERTEX_POINT('',#10721);
#3280=VERTEX_POINT('',#10724);
#3281=VERTEX_POINT('',#10732);
#3282=VERTEX_POINT('',#10733);
#3283=VERTEX_POINT('',#10736);
#3284=VERTEX_POINT('',#10738);
#3285=VERTEX_POINT('',#10742);
#3286=VERTEX_POINT('',#10746);
#3287=VERTEX_POINT('',#10748);
#3288=VERTEX_POINT('',#10752);
#3289=VERTEX_POINT('',#10757);
#3290=VERTEX_POINT('',#10761);
#3291=VERTEX_POINT('',#10767);
#3292=VERTEX_POINT('',#10768);
#3293=VERTEX_POINT('',#10771);
#3294=VERTEX_POINT('',#10773);
#3295=VERTEX_POINT('',#10777);
#3296=VERTEX_POINT('',#10781);
#3297=VERTEX_POINT('',#10783);
#3298=VERTEX_POINT('',#10786);
#3299=VERTEX_POINT('',#10790);
#3300=VERTEX_POINT('',#10794);
#3301=VERTEX_POINT('',#10802);
#3302=VERTEX_POINT('',#10803);
#3303=VERTEX_POINT('',#10806);
#3304=VERTEX_POINT('',#10807);
#3305=VERTEX_POINT('',#10810);
#3306=VERTEX_POINT('',#10811);
#3307=VERTEX_POINT('',#10814);
#3308=VERTEX_POINT('',#10815);
#3309=VERTEX_POINT('',#10818);
#3310=VERTEX_POINT('',#10819);
#3311=VERTEX_POINT('',#10822);
#3312=VERTEX_POINT('',#10823);
#3313=VERTEX_POINT('',#10826);
#3314=VERTEX_POINT('',#10827);
#3315=VERTEX_POINT('',#10830);
#3316=VERTEX_POINT('',#10831);
#3317=VERTEX_POINT('',#10835);
#3318=VERTEX_POINT('',#10836);
#3319=VERTEX_POINT('',#10859);
#3320=VERTEX_POINT('',#10861);
#3321=VERTEX_POINT('',#10886);
#3322=VERTEX_POINT('',#10888);
#3323=VERTEX_POINT('',#10911);
#3324=VERTEX_POINT('',#10913);
#3325=VERTEX_POINT('',#10936);
#3326=VERTEX_POINT('',#10938);
#3327=VERTEX_POINT('',#10951);
#3328=VERTEX_POINT('',#10954);
#3329=VERTEX_POINT('',#10967);
#3330=VERTEX_POINT('',#10969);
#3331=VERTEX_POINT('',#10992);
#3332=VERTEX_POINT('',#10994);
#3333=VERTEX_POINT('',#11017);
#3334=VERTEX_POINT('',#11019);
#3335=VERTEX_POINT('',#11042);
#3336=VERTEX_POINT('',#11044);
#3337=VERTEX_POINT('',#11069);
#3338=VERTEX_POINT('',#11073);
#3339=VERTEX_POINT('',#11098);
#3340=VERTEX_POINT('',#11102);
#3341=VERTEX_POINT('',#11127);
#3342=VERTEX_POINT('',#11131);
#3343=VERTEX_POINT('',#11132);
#3344=VERTEX_POINT('',#11159);
#3345=VERTEX_POINT('',#11163);
#3346=VERTEX_POINT('',#11188);
#3347=VERTEX_POINT('',#11192);
#3348=VERTEX_POINT('',#11217);
#3349=VERTEX_POINT('',#11221);
#3350=VERTEX_POINT('',#11246);
#3351=VERTEX_POINT('',#11249);
#3352=VERTEX_POINT('',#11251);
#3353=VERTEX_POINT('',#11283);
#3354=VERTEX_POINT('',#11285);
#3355=VERTEX_POINT('',#11288);
#3356=VERTEX_POINT('',#11292);
#3357=VERTEX_POINT('',#11297);
#3358=VERTEX_POINT('',#11299);
#3359=VERTEX_POINT('',#11302);
#3360=VERTEX_POINT('',#11306);
#3361=VERTEX_POINT('',#11318);
#3362=VERTEX_POINT('',#11319);
#3363=VERTEX_POINT('',#11321);
#3364=VERTEX_POINT('',#11323);
#3365=VERTEX_POINT('',#11327);
#3366=VERTEX_POINT('',#11329);
#3367=VERTEX_POINT('',#11333);
#3368=VERTEX_POINT('',#11335);
#3369=VERTEX_POINT('',#11343);
#3370=VERTEX_POINT('',#11345);
#3371=VERTEX_POINT('',#11348);
#3372=VERTEX_POINT('',#11352);
#3373=VERTEX_POINT('',#11355);
#3374=VERTEX_POINT('',#11359);
#3375=VERTEX_POINT('',#11362);
#3376=VERTEX_POINT('',#11366);
#3377=VERTEX_POINT('',#11369);
#3378=VERTEX_POINT('',#11373);
#3379=VERTEX_POINT('',#11376);
#3380=VERTEX_POINT('',#11380);
#3381=VERTEX_POINT('',#11386);
#3382=VERTEX_POINT('',#11387);
#3383=VERTEX_POINT('',#11389);
#3384=VERTEX_POINT('',#11391);
#3385=VERTEX_POINT('',#11395);
#3386=VERTEX_POINT('',#11397);
#3387=VERTEX_POINT('',#11401);
#3388=VERTEX_POINT('',#11403);
#3389=VERTEX_POINT('',#11410);
#3390=VERTEX_POINT('',#11412);
#3391=VERTEX_POINT('',#11415);
#3392=VERTEX_POINT('',#11419);
#3393=VERTEX_POINT('',#11427);
#3394=VERTEX_POINT('',#11428);
#3395=VERTEX_POINT('',#11430);
#3396=VERTEX_POINT('',#11432);
#3397=VERTEX_POINT('',#11436);
#3398=VERTEX_POINT('',#11438);
#3399=VERTEX_POINT('',#11442);
#3400=VERTEX_POINT('',#11444);
#3401=VERTEX_POINT('',#11448);
#3402=VERTEX_POINT('',#11450);
#3403=VERTEX_POINT('',#11454);
#3404=VERTEX_POINT('',#11456);
#3405=VERTEX_POINT('',#11465);
#3406=VERTEX_POINT('',#11467);
#3407=VERTEX_POINT('',#11470);
#3408=VERTEX_POINT('',#11475);
#3409=VERTEX_POINT('',#11478);
#3410=VERTEX_POINT('',#11482);
#3411=VERTEX_POINT('',#11486);
#3412=VERTEX_POINT('',#11490);
#3413=VERTEX_POINT('',#11493);
#3414=VERTEX_POINT('',#11497);
#3415=VERTEX_POINT('',#11505);
#3416=VERTEX_POINT('',#11507);
#3417=VERTEX_POINT('',#11511);
#3418=VERTEX_POINT('',#11512);
#3419=VERTEX_POINT('',#11514);
#3420=VERTEX_POINT('',#11516);
#3421=VERTEX_POINT('',#11520);
#3422=VERTEX_POINT('',#11522);
#3423=VERTEX_POINT('',#11524);
#3424=VERTEX_POINT('',#11526);
#3425=VERTEX_POINT('',#11528);
#3426=VERTEX_POINT('',#11530);
#3427=VERTEX_POINT('',#11532);
#3428=VERTEX_POINT('',#11535);
#3429=VERTEX_POINT('',#11538);
#3430=VERTEX_POINT('',#11542);
#3431=VERTEX_POINT('',#11548);
#3432=VERTEX_POINT('',#11550);
#3433=VERTEX_POINT('',#11554);
#3434=VERTEX_POINT('',#11558);
#3435=VERTEX_POINT('',#11564);
#3436=VERTEX_POINT('',#11566);
#3437=VERTEX_POINT('',#11571);
#3438=VERTEX_POINT('',#11573);
#3439=VERTEX_POINT('',#11578);
#3440=VERTEX_POINT('',#11582);
#3441=VERTEX_POINT('',#11589);
#3442=VERTEX_POINT('',#11591);
#3443=VERTEX_POINT('',#11595);
#3444=VERTEX_POINT('',#11597);
#3445=VERTEX_POINT('',#11604);
#3446=VERTEX_POINT('',#11605);
#3447=VERTEX_POINT('',#11609);
#3448=VERTEX_POINT('',#11624);
#3449=VERTEX_POINT('',#11626);
#3450=VERTEX_POINT('',#11628);
#3451=VERTEX_POINT('',#11665);
#3452=VERTEX_POINT('',#11684);
#3453=VERTEX_POINT('',#11686);
#3454=VERTEX_POINT('',#11690);
#3455=VERTEX_POINT('',#11692);
#3456=VERTEX_POINT('',#11699);
#3457=VERTEX_POINT('',#11701);
#3458=VERTEX_POINT('',#11706);
#3459=VERTEX_POINT('',#11708);
#3460=VERTEX_POINT('',#11713);
#3461=VERTEX_POINT('',#11715);
#3462=VERTEX_POINT('',#11718);
#3463=VERTEX_POINT('',#11720);
#3464=VERTEX_POINT('',#11725);
#3465=VERTEX_POINT('',#11729);
#3466=VERTEX_POINT('',#11736);
#3467=VERTEX_POINT('',#11738);
#3468=VERTEX_POINT('',#11742);
#3469=VERTEX_POINT('',#11744);
#3470=VERTEX_POINT('',#11751);
#3471=VERTEX_POINT('',#11753);
#3472=VERTEX_POINT('',#11757);
#3473=VERTEX_POINT('',#11759);
#3474=VERTEX_POINT('',#11766);
#3475=VERTEX_POINT('',#11768);
#3476=VERTEX_POINT('',#11772);
#3477=VERTEX_POINT('',#11774);
#3478=VERTEX_POINT('',#11781);
#3479=VERTEX_POINT('',#11783);
#3480=VERTEX_POINT('',#11787);
#3481=VERTEX_POINT('',#11789);
#3482=VERTEX_POINT('',#11796);
#3483=VERTEX_POINT('',#11799);
#3484=VERTEX_POINT('',#11800);
#3485=VERTEX_POINT('',#11802);
#3486=VERTEX_POINT('',#11804);
#3487=VERTEX_POINT('',#11808);
#3488=VERTEX_POINT('',#11810);
#3489=VERTEX_POINT('',#11814);
#3490=VERTEX_POINT('',#11816);
#3491=VERTEX_POINT('',#11820);
#3492=VERTEX_POINT('',#11822);
#3493=VERTEX_POINT('',#11826);
#3494=VERTEX_POINT('',#11828);
#3495=VERTEX_POINT('',#11836);
#3496=VERTEX_POINT('',#11839);
#3497=VERTEX_POINT('',#11846);
#3498=VERTEX_POINT('',#11847);
#3499=VERTEX_POINT('',#11849);
#3500=VERTEX_POINT('',#11851);
#3501=VERTEX_POINT('',#11855);
#3502=VERTEX_POINT('',#11857);
#3503=VERTEX_POINT('',#11861);
#3504=VERTEX_POINT('',#11863);
#3505=VERTEX_POINT('',#11867);
#3506=VERTEX_POINT('',#11869);
#3507=VERTEX_POINT('',#11873);
#3508=VERTEX_POINT('',#11875);
#3509=VERTEX_POINT('',#11884);
#3510=VERTEX_POINT('',#11887);
#3511=VERTEX_POINT('',#11890);
#3512=VERTEX_POINT('',#11894);
#3513=VERTEX_POINT('',#11898);
#3514=VERTEX_POINT('',#11902);
#3515=VERTEX_POINT('',#11905);
#3516=VERTEX_POINT('',#11912);
#3517=VERTEX_POINT('',#11915);
#3518=VERTEX_POINT('',#11919);
#3519=VERTEX_POINT('',#11923);
#3520=VERTEX_POINT('',#11927);
#3521=VERTEX_POINT('',#11930);
#3522=VERTEX_POINT('',#11934);
#3523=VERTEX_POINT('',#11938);
#3524=VERTEX_POINT('',#11943);
#3525=VERTEX_POINT('',#11944);
#3526=VERTEX_POINT('',#11946);
#3527=VERTEX_POINT('',#11948);
#3528=VERTEX_POINT('',#11952);
#3529=VERTEX_POINT('',#11954);
#3530=VERTEX_POINT('',#11958);
#3531=VERTEX_POINT('',#11960);
#3532=VERTEX_POINT('',#11964);
#3533=VERTEX_POINT('',#11966);
#3534=VERTEX_POINT('',#11970);
#3535=VERTEX_POINT('',#11972);
#3536=VERTEX_POINT('',#12028);
#3537=VERTEX_POINT('',#12030);
#3538=VERTEX_POINT('',#12034);
#3539=VERTEX_POINT('',#12036);
#3540=VERTEX_POINT('',#12040);
#3541=VERTEX_POINT('',#12041);
#3542=VERTEX_POINT('',#12043);
#3543=VERTEX_POINT('',#12045);
#3544=VERTEX_POINT('',#12049);
#3545=VERTEX_POINT('',#12051);
#3546=VERTEX_POINT('',#12055);
#3547=VERTEX_POINT('',#12059);
#3548=VERTEX_POINT('',#12067);
#3549=VERTEX_POINT('',#12069);
#3550=VERTEX_POINT('',#12073);
#3551=VERTEX_POINT('',#12075);
#3552=VERTEX_POINT('',#12082);
#3553=VERTEX_POINT('',#12084);
#3554=VERTEX_POINT('',#12088);
#3555=VERTEX_POINT('',#12090);
#3556=VERTEX_POINT('',#12101);
#3557=VERTEX_POINT('',#12103);
#3558=VERTEX_POINT('',#12108);
#3559=VERTEX_POINT('',#12109);
#3560=VERTEX_POINT('',#12111);
#3561=VERTEX_POINT('',#12113);
#3562=VERTEX_POINT('',#12117);
#3563=VERTEX_POINT('',#12119);
#3564=VERTEX_POINT('',#12121);
#3565=VERTEX_POINT('',#12123);
#3566=VERTEX_POINT('',#12127);
#3567=VERTEX_POINT('',#12131);
#3568=VERTEX_POINT('',#12133);
#3569=VERTEX_POINT('',#12135);
#3570=VERTEX_POINT('',#12139);
#3571=VERTEX_POINT('',#12140);
#3572=VERTEX_POINT('',#12145);
#3573=VERTEX_POINT('',#12147);
#3574=VERTEX_POINT('',#12153);
#3575=VERTEX_POINT('',#12158);
#3576=VERTEX_POINT('',#12162);
#3577=VERTEX_POINT('',#12168);
#3578=VERTEX_POINT('',#12169);
#3579=VERTEX_POINT('',#12173);
#3580=VERTEX_POINT('',#12184);
#3581=VERTEX_POINT('',#12186);
#3582=VERTEX_POINT('',#12189);
#3583=VERTEX_POINT('',#12204);
#3584=VERTEX_POINT('',#12206);
#3585=VERTEX_POINT('',#12210);
#3586=VERTEX_POINT('',#12211);
#3587=VERTEX_POINT('',#12213);
#3588=VERTEX_POINT('',#12215);
#3589=VERTEX_POINT('',#12219);
#3590=VERTEX_POINT('',#12220);
#3591=VERTEX_POINT('',#12225);
#3592=VERTEX_POINT('',#12229);
#3593=VERTEX_POINT('',#12237);
#3594=VERTEX_POINT('',#12239);
#3595=VERTEX_POINT('',#12242);
#3596=VERTEX_POINT('',#12247);
#3597=VERTEX_POINT('',#12253);
#3598=VERTEX_POINT('',#12255);
#3599=VERTEX_POINT('',#12262);
#3600=VERTEX_POINT('',#12263);
#3601=VERTEX_POINT('',#12265);
#3602=VERTEX_POINT('',#12267);
#3603=VERTEX_POINT('',#12271);
#3604=VERTEX_POINT('',#12273);
#3605=VERTEX_POINT('',#12277);
#3606=VERTEX_POINT('',#12279);
#3607=VERTEX_POINT('',#12283);
#3608=VERTEX_POINT('',#12285);
#3609=VERTEX_POINT('',#12289);
#3610=VERTEX_POINT('',#12291);
#3611=VERTEX_POINT('',#12299);
#3612=VERTEX_POINT('',#12302);
#3613=VERTEX_POINT('',#12306);
#3614=VERTEX_POINT('',#12310);
#3615=EDGE_CURVE('',#3074,#3074,#2733,.T.);
#3616=EDGE_CURVE('',#3074,#3075,#1851,.T.);
#3617=EDGE_CURVE('',#3075,#3075,#2734,.T.);
#3618=EDGE_CURVE('',#3076,#3076,#2735,.T.);
#3619=EDGE_CURVE('',#3076,#3077,#1852,.T.);
#3620=EDGE_CURVE('',#3077,#3077,#2736,.T.);
#3621=EDGE_CURVE('',#3078,#3078,#2737,.T.);
#3622=EDGE_CURVE('',#3078,#3079,#1853,.T.);
#3623=EDGE_CURVE('',#3079,#3079,#2738,.T.);
#3624=EDGE_CURVE('',#3080,#3080,#2739,.T.);
#3625=EDGE_CURVE('',#3080,#3081,#1854,.T.);
#3626=EDGE_CURVE('',#3081,#3081,#2740,.T.);
#3627=EDGE_CURVE('',#3082,#3082,#2741,.T.);
#3628=EDGE_CURVE('',#3082,#3083,#1855,.T.);
#3629=EDGE_CURVE('',#3083,#3083,#2742,.T.);
#3630=EDGE_CURVE('',#3084,#3084,#2743,.T.);
#3631=EDGE_CURVE('',#3084,#3085,#1856,.T.);
#3632=EDGE_CURVE('',#3085,#3085,#2744,.T.);
#3633=EDGE_CURVE('',#3086,#3086,#2745,.T.);
#3634=EDGE_CURVE('',#3086,#3087,#1857,.T.);
#3635=EDGE_CURVE('',#3087,#3087,#2746,.T.);
#3636=EDGE_CURVE('',#3088,#3088,#2747,.T.);
#3637=EDGE_CURVE('',#3088,#3089,#1858,.T.);
#3638=EDGE_CURVE('',#3089,#3089,#2748,.T.);
#3639=EDGE_CURVE('',#3090,#3091,#1859,.T.);
#3640=EDGE_CURVE('',#3091,#3092,#1860,.T.);
#3641=EDGE_CURVE('',#3093,#3092,#1861,.T.);
#3642=EDGE_CURVE('',#3090,#3093,#1862,.T.);
#3643=EDGE_CURVE('',#3094,#3090,#1863,.T.);
#3644=EDGE_CURVE('',#3095,#3093,#1864,.T.);
#3645=EDGE_CURVE('',#3094,#3095,#1865,.T.);
#3646=EDGE_CURVE('',#3096,#3094,#1866,.T.);
#3647=EDGE_CURVE('',#3097,#3095,#1867,.T.);
#3648=EDGE_CURVE('',#3096,#3097,#1868,.T.);
#3649=EDGE_CURVE('',#3091,#3096,#1869,.T.);
#3650=EDGE_CURVE('',#3092,#3097,#1870,.T.);
#3651=EDGE_CURVE('',#3098,#3099,#1871,.T.);
#3652=EDGE_CURVE('',#3099,#3100,#1872,.T.);
#3653=EDGE_CURVE('',#3101,#3100,#1873,.T.);
#3654=EDGE_CURVE('',#3098,#3101,#1874,.T.);
#3655=EDGE_CURVE('',#3102,#3098,#1875,.T.);
#3656=EDGE_CURVE('',#3103,#3101,#1876,.T.);
#3657=EDGE_CURVE('',#3102,#3103,#1877,.T.);
#3658=EDGE_CURVE('',#3104,#3102,#1878,.T.);
#3659=EDGE_CURVE('',#3105,#3103,#1879,.T.);
#3660=EDGE_CURVE('',#3104,#3105,#1880,.T.);
#3661=EDGE_CURVE('',#3099,#3104,#1881,.T.);
#3662=EDGE_CURVE('',#3100,#3105,#1882,.T.);
#3663=EDGE_CURVE('',#3106,#3107,#1883,.T.);
#3664=EDGE_CURVE('',#3107,#3108,#1884,.T.);
#3665=EDGE_CURVE('',#3109,#3108,#1885,.T.);
#3666=EDGE_CURVE('',#3106,#3109,#1886,.T.);
#3667=EDGE_CURVE('',#3110,#3106,#1887,.T.);
#3668=EDGE_CURVE('',#3111,#3109,#1888,.T.);
#3669=EDGE_CURVE('',#3110,#3111,#1889,.T.);
#3670=EDGE_CURVE('',#3112,#3110,#1890,.T.);
#3671=EDGE_CURVE('',#3113,#3111,#1891,.T.);
#3672=EDGE_CURVE('',#3112,#3113,#1892,.T.);
#3673=EDGE_CURVE('',#3107,#3112,#1893,.T.);
#3674=EDGE_CURVE('',#3108,#3113,#1894,.T.);
#3675=EDGE_CURVE('',#3114,#3114,#2749,.T.);
#3676=EDGE_CURVE('',#3114,#3115,#1895,.T.);
#3677=EDGE_CURVE('',#3115,#3115,#2750,.T.);
#3678=EDGE_CURVE('',#3116,#3116,#2751,.T.);
#3679=EDGE_CURVE('',#3116,#3117,#1896,.T.);
#3680=EDGE_CURVE('',#3117,#3117,#2752,.T.);
#3681=EDGE_CURVE('',#3118,#3118,#2753,.T.);
#3682=EDGE_CURVE('',#3118,#3119,#1897,.T.);
#3683=EDGE_CURVE('',#3119,#3119,#2754,.T.);
#3684=EDGE_CURVE('',#3120,#3120,#2755,.T.);
#3685=EDGE_CURVE('',#3120,#3121,#1898,.T.);
#3686=EDGE_CURVE('',#3121,#3121,#2756,.T.);
#3687=EDGE_CURVE('',#3122,#3122,#2757,.T.);
#3688=EDGE_CURVE('',#3122,#3123,#1899,.T.);
#3689=EDGE_CURVE('',#3123,#3123,#2758,.T.);
#3690=EDGE_CURVE('',#3124,#3124,#2759,.T.);
#3691=EDGE_CURVE('',#3124,#3125,#1900,.T.);
#3692=EDGE_CURVE('',#3125,#3125,#2760,.T.);
#3693=EDGE_CURVE('',#3126,#3126,#2761,.T.);
#3694=EDGE_CURVE('',#3126,#3127,#1901,.T.);
#3695=EDGE_CURVE('',#3127,#3127,#2762,.T.);
#3696=EDGE_CURVE('',#3128,#3128,#2763,.T.);
#3697=EDGE_CURVE('',#3128,#3129,#1902,.T.);
#3698=EDGE_CURVE('',#3129,#3129,#2764,.T.);
#3699=EDGE_CURVE('',#3130,#3130,#2765,.T.);
#3700=EDGE_CURVE('',#3130,#3131,#1903,.T.);
#3701=EDGE_CURVE('',#3131,#3131,#2766,.T.);
#3702=EDGE_CURVE('',#3132,#3132,#2767,.T.);
#3703=EDGE_CURVE('',#3132,#3133,#1904,.T.);
#3704=EDGE_CURVE('',#3133,#3133,#2768,.T.);
#3705=EDGE_CURVE('',#3134,#3134,#2769,.T.);
#3706=EDGE_CURVE('',#3134,#3135,#1905,.T.);
#3707=EDGE_CURVE('',#3135,#3135,#2770,.T.);
#3708=EDGE_CURVE('',#3136,#3136,#2771,.T.);
#3709=EDGE_CURVE('',#3136,#3137,#1906,.T.);
#3710=EDGE_CURVE('',#3137,#3137,#2772,.T.);
#3711=EDGE_CURVE('',#3138,#3138,#2773,.T.);
#3712=EDGE_CURVE('',#3138,#3139,#1907,.T.);
#3713=EDGE_CURVE('',#3139,#3139,#2774,.T.);
#3714=EDGE_CURVE('',#3140,#3140,#2775,.T.);
#3715=EDGE_CURVE('',#3140,#3141,#1908,.T.);
#3716=EDGE_CURVE('',#3141,#3141,#2776,.T.);
#3717=EDGE_CURVE('',#3142,#3142,#2777,.T.);
#3718=EDGE_CURVE('',#3143,#3143,#2778,.T.);
#3719=EDGE_CURVE('',#3143,#3142,#1909,.T.);
#3720=EDGE_CURVE('',#3144,#3144,#2779,.T.);
#3721=EDGE_CURVE('',#3144,#3145,#1910,.T.);
#3722=EDGE_CURVE('',#3145,#3145,#2780,.T.);
#3723=EDGE_CURVE('',#3146,#3147,#1911,.T.);
#3724=EDGE_CURVE('',#3146,#3148,#2781,.T.);
#3725=EDGE_CURVE('',#3149,#3148,#1912,.T.);
#3726=EDGE_CURVE('',#3147,#3149,#2782,.T.);
#3727=EDGE_CURVE('',#3147,#3150,#1913,.T.);
#3728=EDGE_CURVE('',#3150,#3151,#1914,.T.);
#3729=EDGE_CURVE('',#3152,#3151,#1915,.T.);
#3730=EDGE_CURVE('',#3153,#3152,#1916,.T.);
#3731=EDGE_CURVE('',#3153,#3154,#1917,.T.);
#3732=EDGE_CURVE('',#3154,#3155,#1918,.T.);
#3733=EDGE_CURVE('',#3155,#3156,#1919,.T.);
#3734=EDGE_CURVE('',#3157,#3156,#2783,.T.);
#3735=EDGE_CURVE('',#3157,#3146,#1920,.T.);
#3736=EDGE_CURVE('',#3158,#3149,#1921,.T.);
#3737=EDGE_CURVE('',#3150,#3158,#1922,.T.);
#3738=EDGE_CURVE('',#3159,#3160,#1923,.T.);
#3739=EDGE_CURVE('',#3160,#3161,#1924,.T.);
#3740=EDGE_CURVE('',#3161,#3162,#1925,.T.);
#3741=EDGE_CURVE('',#3162,#3159,#1926,.T.);
#3742=EDGE_CURVE('',#3163,#3164,#1927,.T.);
#3743=EDGE_CURVE('',#3154,#3163,#1928,.T.);
#3744=EDGE_CURVE('',#3164,#3153,#1929,.T.);
#3745=EDGE_CURVE('',#3165,#3166,#1930,.T.);
#3746=EDGE_CURVE('',#3166,#3159,#1931,.T.);
#3747=EDGE_CURVE('',#3165,#3162,#1932,.T.);
#3748=EDGE_CURVE('',#3167,#3165,#1933,.T.);
#3749=EDGE_CURVE('',#3167,#3161,#1934,.T.);
#3750=EDGE_CURVE('',#3168,#3167,#1935,.T.);
#3751=EDGE_CURVE('',#3168,#3160,#1936,.T.);
#3752=EDGE_CURVE('',#3166,#3168,#1937,.T.);
#3753=EDGE_CURVE('',#3163,#3169,#1938,.T.);
#3754=EDGE_CURVE('',#3169,#3155,#1939,.T.);
#3755=EDGE_CURVE('',#3157,#3170,#1940,.T.);
#3756=EDGE_CURVE('',#3171,#3156,#1941,.T.);
#3757=EDGE_CURVE('',#3170,#3171,#2784,.T.);
#3758=EDGE_CURVE('',#3148,#3170,#1942,.T.);
#3759=EDGE_CURVE('',#3171,#3169,#1943,.T.);
#3760=EDGE_CURVE('',#3164,#3172,#1944,.T.);
#3761=EDGE_CURVE('',#3173,#3172,#1945,.T.);
#3762=EDGE_CURVE('',#3158,#3173,#1946,.T.);
#3763=EDGE_CURVE('',#3151,#3173,#1947,.T.);
#3764=EDGE_CURVE('',#3172,#3152,#1948,.T.);
#3765=EDGE_CURVE('',#3174,#3174,#2785,.T.);
#3766=EDGE_CURVE('',#3174,#3175,#1949,.T.);
#3767=EDGE_CURVE('',#3175,#3175,#2786,.T.);
#3768=EDGE_CURVE('',#3176,#3176,#2787,.T.);
#3769=EDGE_CURVE('',#3176,#3177,#1950,.T.);
#3770=EDGE_CURVE('',#3177,#3177,#2788,.T.);
#3771=EDGE_CURVE('',#3178,#3178,#2789,.T.);
#3772=EDGE_CURVE('',#3178,#3179,#1951,.T.);
#3773=EDGE_CURVE('',#3179,#3179,#2790,.T.);
#3774=EDGE_CURVE('',#3180,#3180,#2791,.T.);
#3775=EDGE_CURVE('',#3180,#3181,#1952,.T.);
#3776=EDGE_CURVE('',#3181,#3181,#2792,.T.);
#3777=EDGE_CURVE('',#3182,#3182,#2793,.T.);
#3778=EDGE_CURVE('',#3182,#3183,#1953,.T.);
#3779=EDGE_CURVE('',#3183,#3183,#2794,.T.);
#3780=EDGE_CURVE('',#3184,#3184,#2795,.T.);
#3781=EDGE_CURVE('',#3184,#3185,#1954,.T.);
#3782=EDGE_CURVE('',#3185,#3185,#2796,.T.);
#3783=EDGE_CURVE('',#3186,#3186,#2797,.T.);
#3784=EDGE_CURVE('',#3186,#3187,#1955,.T.);
#3785=EDGE_CURVE('',#3187,#3187,#2798,.T.);
#3786=EDGE_CURVE('',#3188,#3188,#2799,.T.);
#3787=EDGE_CURVE('',#3188,#3189,#1956,.T.);
#3788=EDGE_CURVE('',#3189,#3189,#2800,.T.);
#3789=EDGE_CURVE('',#3190,#3190,#2801,.T.);
#3790=EDGE_CURVE('',#3190,#3191,#1957,.T.);
#3791=EDGE_CURVE('',#3191,#3191,#2802,.T.);
#3792=EDGE_CURVE('',#3192,#3192,#2803,.T.);
#3793=EDGE_CURVE('',#3192,#3193,#1958,.T.);
#3794=EDGE_CURVE('',#3193,#3193,#2804,.T.);
#3795=EDGE_CURVE('',#3194,#3194,#2805,.T.);
#3796=EDGE_CURVE('',#3194,#3195,#1959,.T.);
#3797=EDGE_CURVE('',#3195,#3195,#2806,.T.);
#3798=EDGE_CURVE('',#3196,#3196,#2807,.T.);
#3799=EDGE_CURVE('',#3196,#3197,#1960,.T.);
#3800=EDGE_CURVE('',#3197,#3197,#2808,.T.);
#3801=EDGE_CURVE('',#3198,#3198,#2809,.T.);
#3802=EDGE_CURVE('',#3199,#3199,#2810,.T.);
#3803=EDGE_CURVE('',#3199,#3198,#1961,.T.);
#3804=EDGE_CURVE('',#3200,#3200,#2811,.T.);
#3805=EDGE_CURVE('',#3200,#3201,#1962,.T.);
#3806=EDGE_CURVE('',#3201,#3201,#2812,.T.);
#3807=EDGE_CURVE('',#3202,#3202,#2813,.T.);
#3808=EDGE_CURVE('',#3202,#3203,#1963,.T.);
#3809=EDGE_CURVE('',#3203,#3203,#2814,.T.);
#3810=EDGE_CURVE('',#3204,#3204,#2815,.T.);
#3811=EDGE_CURVE('',#3205,#3205,#2816,.T.);
#3812=EDGE_CURVE('',#3205,#3206,#1964,.T.);
#3813=EDGE_CURVE('',#3206,#3206,#2817,.T.);
#3814=EDGE_CURVE('',#3207,#3207,#2818,.T.);
#3815=EDGE_CURVE('',#3208,#3208,#2819,.T.);
#3816=EDGE_CURVE('',#3208,#3209,#1965,.T.);
#3817=EDGE_CURVE('',#3209,#3209,#2820,.T.);
#3818=EDGE_CURVE('',#3210,#3210,#2821,.T.);
#3819=EDGE_CURVE('',#3211,#3211,#2822,.T.);
#3820=EDGE_CURVE('',#3211,#3212,#1966,.T.);
#3821=EDGE_CURVE('',#3212,#3212,#2823,.T.);
#3822=EDGE_CURVE('',#3213,#3213,#2824,.T.);
#3823=EDGE_CURVE('',#3214,#3214,#2825,.T.);
#3824=EDGE_CURVE('',#3214,#3204,#1967,.T.);
#3825=EDGE_CURVE('',#3215,#3215,#2826,.T.);
#3826=EDGE_CURVE('',#3215,#3207,#1968,.T.);
#3827=EDGE_CURVE('',#3216,#3216,#2827,.T.);
#3828=EDGE_CURVE('',#3216,#3210,#1969,.T.);
#3829=EDGE_CURVE('',#3217,#3217,#2828,.T.);
#3830=EDGE_CURVE('',#3217,#3213,#1970,.T.);
#3831=EDGE_CURVE('',#3218,#3218,#2829,.T.);
#3832=EDGE_CURVE('',#3218,#3219,#1971,.T.);
#3833=EDGE_CURVE('',#3219,#3219,#2830,.T.);
#3834=EDGE_CURVE('',#3220,#3220,#2831,.T.);
#3835=EDGE_CURVE('',#3221,#3221,#2832,.T.);
#3836=EDGE_CURVE('',#3221,#3220,#1972,.T.);
#3837=EDGE_CURVE('',#3222,#3222,#2833,.T.);
#3838=EDGE_CURVE('',#3222,#3223,#1973,.T.);
#3839=EDGE_CURVE('',#3223,#3223,#2834,.T.);
#3840=EDGE_CURVE('',#3224,#3225,#1974,.T.);
#3841=EDGE_CURVE('',#3225,#3226,#1975,.T.);
#3842=EDGE_CURVE('',#3227,#3226,#1976,.T.);
#3843=EDGE_CURVE('',#3224,#3227,#1977,.T.);
#3844=EDGE_CURVE('',#3228,#3224,#1978,.T.);
#3845=EDGE_CURVE('',#3229,#3227,#1979,.T.);
#3846=EDGE_CURVE('',#3228,#3229,#1980,.T.);
#3847=EDGE_CURVE('',#3230,#3228,#1981,.T.);
#3848=EDGE_CURVE('',#3231,#3229,#1982,.T.);
#3849=EDGE_CURVE('',#3230,#3231,#1983,.T.);
#3850=EDGE_CURVE('',#3225,#3230,#1984,.T.);
#3851=EDGE_CURVE('',#3226,#3231,#1985,.T.);
#3852=EDGE_CURVE('',#3232,#3232,#2835,.T.);
#3853=EDGE_CURVE('',#3232,#3233,#1986,.T.);
#3854=EDGE_CURVE('',#3233,#3233,#2836,.T.);
#3855=EDGE_CURVE('',#3234,#3234,#2837,.T.);
#3856=EDGE_CURVE('',#3234,#3235,#1987,.T.);
#3857=EDGE_CURVE('',#3235,#3235,#2838,.T.);
#3858=EDGE_CURVE('',#3236,#3237,#1988,.T.);
#3859=EDGE_CURVE('',#3237,#3238,#1989,.T.);
#3860=EDGE_CURVE('',#3239,#3238,#1990,.T.);
#3861=EDGE_CURVE('',#3236,#3239,#1991,.T.);
#3862=EDGE_CURVE('',#3240,#3236,#1992,.T.);
#3863=EDGE_CURVE('',#3241,#3239,#1993,.T.);
#3864=EDGE_CURVE('',#3240,#3241,#1994,.T.);
#3865=EDGE_CURVE('',#3242,#3240,#1995,.T.);
#3866=EDGE_CURVE('',#3243,#3241,#1996,.T.);
#3867=EDGE_CURVE('',#3242,#3243,#1997,.T.);
#3868=EDGE_CURVE('',#3237,#3242,#1998,.T.);
#3869=EDGE_CURVE('',#3238,#3243,#1999,.T.);
#3870=EDGE_CURVE('',#3244,#3244,#2839,.T.);
#3871=EDGE_CURVE('',#3244,#3245,#2000,.T.);
#3872=EDGE_CURVE('',#3245,#3245,#2840,.T.);
#3873=EDGE_CURVE('',#3246,#3246,#2841,.T.);
#3874=EDGE_CURVE('',#3246,#3247,#2001,.T.);
#3875=EDGE_CURVE('',#3247,#3247,#2842,.T.);
#3876=EDGE_CURVE('',#3248,#3249,#2002,.T.);
#3877=EDGE_CURVE('',#3249,#3250,#2003,.T.);
#3878=EDGE_CURVE('',#3251,#3250,#2004,.T.);
#3879=EDGE_CURVE('',#3248,#3251,#2005,.T.);
#3880=EDGE_CURVE('',#3252,#3248,#2006,.T.);
#3881=EDGE_CURVE('',#3253,#3251,#2007,.T.);
#3882=EDGE_CURVE('',#3252,#3253,#2008,.T.);
#3883=EDGE_CURVE('',#3254,#3252,#2009,.T.);
#3884=EDGE_CURVE('',#3255,#3253,#2010,.T.);
#3885=EDGE_CURVE('',#3254,#3255,#2011,.T.);
#3886=EDGE_CURVE('',#3249,#3254,#2012,.T.);
#3887=EDGE_CURVE('',#3250,#3255,#2013,.T.);
#3888=EDGE_CURVE('',#3256,#3256,#2843,.T.);
#3889=EDGE_CURVE('',#3256,#3257,#2014,.T.);
#3890=EDGE_CURVE('',#3257,#3257,#2844,.T.);
#3891=EDGE_CURVE('',#3258,#3258,#2845,.T.);
#3892=EDGE_CURVE('',#3259,#3259,#2846,.T.);
#3893=EDGE_CURVE('',#3260,#3260,#2847,.T.);
#3894=EDGE_CURVE('',#3260,#3258,#2015,.T.);
#3895=EDGE_CURVE('',#3259,#3261,#2016,.T.);
#3896=EDGE_CURVE('',#3261,#3261,#2848,.T.);
#3897=EDGE_CURVE('',#3262,#3263,#2017,.T.);
#3898=EDGE_CURVE('',#3263,#3264,#2018,.T.);
#3899=EDGE_CURVE('',#3264,#3265,#2019,.T.);
#3900=EDGE_CURVE('',#3262,#3265,#2020,.T.);
#3901=EDGE_CURVE('',#3263,#3266,#2021,.T.);
#3902=EDGE_CURVE('',#3266,#3267,#2022,.T.);
#3903=EDGE_CURVE('',#3267,#3264,#2023,.T.);
#3904=EDGE_CURVE('',#3266,#3268,#2024,.T.);
#3905=EDGE_CURVE('',#3268,#3269,#2025,.T.);
#3906=EDGE_CURVE('',#3269,#3267,#2026,.T.);
#3907=EDGE_CURVE('',#3268,#3270,#2027,.T.);
#3908=EDGE_CURVE('',#3270,#3271,#2028,.T.);
#3909=EDGE_CURVE('',#3271,#3269,#2029,.T.);
#3910=EDGE_CURVE('',#3270,#3272,#2030,.T.);
#3911=EDGE_CURVE('',#3272,#3273,#2031,.T.);
#3912=EDGE_CURVE('',#3273,#3271,#2032,.T.);
#3913=EDGE_CURVE('',#3272,#3262,#2033,.T.);
#3914=EDGE_CURVE('',#3265,#3273,#2034,.T.);
#3915=EDGE_CURVE('',#3274,#3274,#2849,.T.);
#3916=EDGE_CURVE('',#3275,#3275,#2850,.T.);
#3917=EDGE_CURVE('',#3276,#3276,#2851,.T.);
#3918=EDGE_CURVE('',#3276,#3275,#2035,.T.);
#3919=EDGE_CURVE('',#3277,#3277,#2852,.T.);
#3920=EDGE_CURVE('',#3277,#3276,#2036,.T.);
#3921=EDGE_CURVE('',#3278,#3278,#2853,.T.);
#3922=EDGE_CURVE('',#3278,#3277,#2037,.T.);
#3923=EDGE_CURVE('',#3279,#3279,#2854,.T.);
#3924=EDGE_CURVE('',#3280,#3280,#2855,.F.);
#3925=EDGE_CURVE('',#3280,#3279,#2038,.T.);
#3926=EDGE_CURVE('',#3274,#3280,#2039,.T.);
#3927=EDGE_CURVE('',#3281,#3282,#2856,.T.);
#3928=EDGE_CURVE('',#3282,#3281,#2857,.T.);
#3929=EDGE_CURVE('',#3282,#3283,#2858,.T.);
#3930=EDGE_CURVE('',#3284,#3283,#2859,.T.);
#3931=EDGE_CURVE('',#3283,#3284,#2860,.T.);
#3932=EDGE_CURVE('',#3284,#3285,#2040,.T.);
#3933=EDGE_CURVE('',#3285,#3285,#2861,.T.);
#3934=EDGE_CURVE('',#3286,#3286,#2862,.T.);
#3935=EDGE_CURVE('',#3286,#3287,#2041,.T.);
#3936=EDGE_CURVE('',#3287,#3287,#2863,.T.);
#3937=EDGE_CURVE('',#3287,#3288,#2042,.T.);
#3938=EDGE_CURVE('',#3288,#3288,#2864,.T.);
#3939=EDGE_CURVE('',#3289,#3289,#2865,.T.);
#3940=EDGE_CURVE('',#3289,#3281,#2043,.T.);
#3941=EDGE_CURVE('',#3290,#3290,#2866,.T.);
#3942=EDGE_CURVE('',#3290,#3286,#2044,.T.);
#3943=EDGE_CURVE('',#3291,#3292,#2867,.T.);
#3944=EDGE_CURVE('',#3292,#3291,#2868,.T.);
#3945=EDGE_CURVE('',#3292,#3293,#2869,.T.);
#3946=EDGE_CURVE('',#3294,#3293,#2870,.T.);
#3947=EDGE_CURVE('',#3293,#3294,#2871,.T.);
#3948=EDGE_CURVE('',#3295,#3295,#2872,.T.);
#3949=EDGE_CURVE('',#3295,#3294,#2045,.T.);
#3950=EDGE_CURVE('',#3296,#3296,#2873,.T.);
#3951=EDGE_CURVE('',#3297,#3297,#2874,.T.);
#3952=EDGE_CURVE('',#3298,#3298,#2875,.T.);
#3953=EDGE_CURVE('',#3298,#3296,#2046,.T.);
#3954=EDGE_CURVE('',#3299,#3299,#2876,.T.);
#3955=EDGE_CURVE('',#3299,#3298,#2047,.T.);
#3956=EDGE_CURVE('',#3300,#3300,#2877,.T.);
#3957=EDGE_CURVE('',#3300,#3299,#2048,.T.);
#3958=EDGE_CURVE('',#3291,#3297,#2049,.T.);
#3959=EDGE_CURVE('',#3301,#3302,#2878,.T.);
#3960=EDGE_CURVE('',#3303,#3304,#2879,.T.);
#3961=EDGE_CURVE('',#3305,#3306,#2880,.T.);
#3962=EDGE_CURVE('',#3307,#3308,#2881,.T.);
#3963=EDGE_CURVE('',#3309,#3310,#2882,.T.);
#3964=EDGE_CURVE('',#3311,#3312,#2883,.T.);
#3965=EDGE_CURVE('',#3313,#3314,#2884,.T.);
#3966=EDGE_CURVE('',#3315,#3316,#2885,.T.);
#3967=EDGE_CURVE('',#3317,#3318,#263,.T.);
#3968=EDGE_CURVE('',#3319,#3317,#2886,.T.);
#3969=EDGE_CURVE('',#3320,#3319,#264,.T.);
#3970=EDGE_CURVE('',#3318,#3320,#2887,.T.);
#3971=EDGE_CURVE('',#3321,#3319,#2888,.T.);
#3972=EDGE_CURVE('',#3321,#3322,#265,.T.);
#3973=EDGE_CURVE('',#3323,#3322,#2889,.T.);
#3974=EDGE_CURVE('',#3323,#3324,#266,.T.);
#3975=EDGE_CURVE('',#3325,#3324,#2890,.T.);
#3976=EDGE_CURVE('',#3325,#3326,#267,.T.);
#3977=EDGE_CURVE('',#3326,#3327,#2050,.T.);
#3978=EDGE_CURVE('',#3327,#3327,#2891,.T.);
#3979=EDGE_CURVE('',#3326,#3328,#268,.T.);
#3980=EDGE_CURVE('',#3329,#3328,#2892,.T.);
#3981=EDGE_CURVE('',#3329,#3330,#269,.T.);
#3982=EDGE_CURVE('',#3331,#3330,#2893,.T.);
#3983=EDGE_CURVE('',#3331,#3332,#270,.T.);
#3984=EDGE_CURVE('',#3333,#3332,#2894,.T.);
#3985=EDGE_CURVE('',#3333,#3334,#271,.T.);
#3986=EDGE_CURVE('',#3335,#3334,#2895,.T.);
#3987=EDGE_CURVE('',#3335,#3336,#272,.T.);
#3988=EDGE_CURVE('',#3320,#3336,#2896,.T.);
#3989=EDGE_CURVE('',#3317,#3337,#2897,.T.);
#3990=EDGE_CURVE('',#3337,#3321,#2898,.T.);
#3991=EDGE_CURVE('',#3338,#3337,#273,.T.);
#3992=EDGE_CURVE('',#3322,#3338,#2899,.T.);
#3993=EDGE_CURVE('',#3338,#3339,#2900,.T.);
#3994=EDGE_CURVE('',#3339,#3323,#2901,.T.);
#3995=EDGE_CURVE('',#3340,#3339,#274,.T.);
#3996=EDGE_CURVE('',#3324,#3340,#2902,.T.);
#3997=EDGE_CURVE('',#3340,#3341,#2903,.T.);
#3998=EDGE_CURVE('',#3341,#3325,#2904,.T.);
#3999=EDGE_CURVE('',#3342,#3343,#275,.T.);
#4000=EDGE_CURVE('',#3328,#3342,#2905,.T.);
#4001=EDGE_CURVE('',#3343,#3341,#276,.T.);
#4002=EDGE_CURVE('',#3342,#3344,#2906,.T.);
#4003=EDGE_CURVE('',#3344,#3329,#2907,.T.);
#4004=EDGE_CURVE('',#3345,#3344,#277,.T.);
#4005=EDGE_CURVE('',#3330,#3345,#2908,.T.);
#4006=EDGE_CURVE('',#3345,#3346,#2909,.T.);
#4007=EDGE_CURVE('',#3346,#3331,#2910,.T.);
#4008=EDGE_CURVE('',#3347,#3346,#278,.T.);
#4009=EDGE_CURVE('',#3332,#3347,#2911,.T.);
#4010=EDGE_CURVE('',#3347,#3348,#2912,.T.);
#4011=EDGE_CURVE('',#3348,#3333,#2913,.T.);
#4012=EDGE_CURVE('',#3349,#3348,#279,.T.);
#4013=EDGE_CURVE('',#3334,#3349,#2914,.T.);
#4014=EDGE_CURVE('',#3350,#3350,#2915,.T.);
#4015=EDGE_CURVE('',#3350,#3343,#2051,.T.);
#4016=EDGE_CURVE('',#3351,#3318,#2916,.T.);
#4017=EDGE_CURVE('',#3351,#3352,#280,.T.);
#4018=EDGE_CURVE('',#3349,#3352,#2917,.T.);
#4019=EDGE_CURVE('',#3336,#3351,#2918,.T.);
#4020=EDGE_CURVE('',#3352,#3335,#2919,.T.);
#4021=EDGE_CURVE('',#3353,#3353,#2920,.T.);
#4022=EDGE_CURVE('',#3354,#3354,#2921,.T.);
#4023=EDGE_CURVE('',#3355,#3355,#2922,.T.);
#4024=EDGE_CURVE('',#3355,#3353,#2052,.T.);
#4025=EDGE_CURVE('',#3356,#3356,#2923,.T.);
#4026=EDGE_CURVE('',#3356,#3354,#2053,.T.);
#4027=EDGE_CURVE('',#3357,#3357,#2924,.T.);
#4028=EDGE_CURVE('',#3358,#3358,#2925,.T.);
#4029=EDGE_CURVE('',#3359,#3359,#2926,.T.);
#4030=EDGE_CURVE('',#3359,#3357,#2054,.T.);
#4031=EDGE_CURVE('',#3360,#3360,#2927,.T.);
#4032=EDGE_CURVE('',#3360,#3358,#2055,.T.);
#4033=EDGE_CURVE('',#3361,#3362,#2928,.T.);
#4034=EDGE_CURVE('',#3363,#3361,#2056,.T.);
#4035=EDGE_CURVE('',#3364,#3363,#2057,.T.);
#4036=EDGE_CURVE('',#3362,#3364,#2058,.T.);
#4037=EDGE_CURVE('',#3362,#3365,#2059,.T.);
#4038=EDGE_CURVE('',#3366,#3364,#2060,.T.);
#4039=EDGE_CURVE('',#3366,#3365,#2061,.T.);
#4040=EDGE_CURVE('',#3365,#3367,#2929,.T.);
#4041=EDGE_CURVE('',#3368,#3366,#2062,.T.);
#4042=EDGE_CURVE('',#3367,#3368,#2063,.T.);
#4043=EDGE_CURVE('',#3367,#3361,#2064,.T.);
#4044=EDGE_CURVE('',#3368,#3363,#2065,.T.);
#4045=EDGE_CURVE('',#3369,#3369,#2930,.T.);
#4046=EDGE_CURVE('',#3370,#3370,#2931,.T.);
#4047=EDGE_CURVE('',#3371,#3371,#2932,.T.);
#4048=EDGE_CURVE('',#3371,#3369,#2066,.T.);
#4049=EDGE_CURVE('',#3372,#3372,#2933,.T.);
#4050=EDGE_CURVE('',#3373,#3373,#2934,.T.);
#4051=EDGE_CURVE('',#3373,#3372,#2067,.T.);
#4052=EDGE_CURVE('',#3374,#3374,#2935,.T.);
#4053=EDGE_CURVE('',#3375,#3375,#2936,.T.);
#4054=EDGE_CURVE('',#3375,#3374,#2068,.T.);
#4055=EDGE_CURVE('',#3376,#3376,#2937,.T.);
#4056=EDGE_CURVE('',#3377,#3377,#2938,.T.);
#4057=EDGE_CURVE('',#3377,#3376,#2069,.T.);
#4058=EDGE_CURVE('',#3378,#3378,#2939,.T.);
#4059=EDGE_CURVE('',#3379,#3379,#2940,.T.);
#4060=EDGE_CURVE('',#3379,#3378,#2070,.T.);
#4061=EDGE_CURVE('',#3380,#3380,#2941,.T.);
#4062=EDGE_CURVE('',#3380,#3370,#2071,.T.);
#4063=EDGE_CURVE('',#3381,#3382,#2942,.T.);
#4064=EDGE_CURVE('',#3383,#3381,#2072,.T.);
#4065=EDGE_CURVE('',#3384,#3383,#2943,.T.);
#4066=EDGE_CURVE('',#3382,#3384,#2073,.T.);
#4067=EDGE_CURVE('',#3382,#3385,#2074,.T.);
#4068=EDGE_CURVE('',#3386,#3384,#2075,.T.);
#4069=EDGE_CURVE('',#3386,#3385,#2076,.T.);
#4070=EDGE_CURVE('',#3385,#3387,#2944,.T.);
#4071=EDGE_CURVE('',#3388,#3386,#2945,.T.);
#4072=EDGE_CURVE('',#3387,#3388,#2077,.T.);
#4073=EDGE_CURVE('',#3387,#3381,#2078,.T.);
#4074=EDGE_CURVE('',#3383,#3388,#2079,.T.);
#4075=EDGE_CURVE('',#3389,#3389,#2946,.T.);
#4076=EDGE_CURVE('',#3390,#3390,#2947,.T.);
#4077=EDGE_CURVE('',#3391,#3391,#2948,.T.);
#4078=EDGE_CURVE('',#3391,#3389,#2080,.T.);
#4079=EDGE_CURVE('',#3392,#3392,#2949,.T.);
#4080=EDGE_CURVE('',#3392,#3390,#2081,.T.);
#4081=EDGE_CURVE('',#3393,#3394,#2082,.T.);
#4082=EDGE_CURVE('',#3394,#3395,#2083,.T.);
#4083=EDGE_CURVE('',#3395,#3396,#2084,.T.);
#4084=EDGE_CURVE('',#3393,#3396,#2085,.T.);
#4085=EDGE_CURVE('',#3394,#3397,#2086,.T.);
#4086=EDGE_CURVE('',#3397,#3398,#2087,.T.);
#4087=EDGE_CURVE('',#3398,#3395,#2088,.T.);
#4088=EDGE_CURVE('',#3397,#3399,#2089,.T.);
#4089=EDGE_CURVE('',#3399,#3400,#2090,.T.);
#4090=EDGE_CURVE('',#3400,#3398,#2091,.T.);
#4091=EDGE_CURVE('',#3399,#3401,#2092,.T.);
#4092=EDGE_CURVE('',#3401,#3402,#2093,.T.);
#4093=EDGE_CURVE('',#3402,#3400,#2094,.T.);
#4094=EDGE_CURVE('',#3401,#3403,#2095,.T.);
#4095=EDGE_CURVE('',#3403,#3404,#2096,.T.);
#4096=EDGE_CURVE('',#3404,#3402,#2097,.T.);
#4097=EDGE_CURVE('',#3403,#3393,#2098,.T.);
#4098=EDGE_CURVE('',#3396,#3404,#2099,.T.);
#4099=EDGE_CURVE('',#3405,#3405,#2950,.T.);
#4100=EDGE_CURVE('',#3406,#3406,#2951,.T.);
#4101=EDGE_CURVE('',#3405,#3407,#2100,.T.);
#4102=EDGE_CURVE('',#3407,#3407,#2952,.T.);
#4103=EDGE_CURVE('',#3408,#3408,#2953,.T.);
#4104=EDGE_CURVE('',#3409,#3409,#2954,.T.);
#4105=EDGE_CURVE('',#3409,#3408,#2101,.T.);
#4106=EDGE_CURVE('',#3410,#3410,#2955,.T.);
#4107=EDGE_CURVE('',#3410,#3409,#2102,.T.);
#4108=EDGE_CURVE('',#3411,#3411,#2956,.T.);
#4109=EDGE_CURVE('',#3411,#3410,#2103,.T.);
#4110=EDGE_CURVE('',#3412,#3412,#2957,.T.);
#4111=EDGE_CURVE('',#3413,#3413,#2958,.F.);
#4112=EDGE_CURVE('',#3413,#3412,#2104,.T.);
#4113=EDGE_CURVE('',#3414,#3414,#2959,.F.);
#4114=EDGE_CURVE('',#3414,#3413,#2105,.T.);
#4115=EDGE_CURVE('',#3406,#3414,#2106,.T.);
#4116=EDGE_CURVE('',#3415,#3415,#2960,.T.);
#4117=EDGE_CURVE('',#3415,#3416,#2107,.T.);
#4118=EDGE_CURVE('',#3416,#3416,#2961,.T.);
#4119=EDGE_CURVE('',#3417,#3418,#2108,.T.);
#4120=EDGE_CURVE('',#3419,#3417,#2962,.T.);
#4121=EDGE_CURVE('',#3420,#3419,#2109,.T.);
#4122=EDGE_CURVE('',#3420,#3418,#2963,.T.);
#4123=EDGE_CURVE('',#3421,#3420,#2110,.T.);
#4124=EDGE_CURVE('',#3422,#3421,#2964,.T.);
#4125=EDGE_CURVE('',#3423,#3422,#2965,.T.);
#4126=EDGE_CURVE('',#3424,#3423,#2111,.T.);
#4127=EDGE_CURVE('',#3425,#3424,#2966,.T.);
#4128=EDGE_CURVE('',#3426,#3425,#2112,.T.);
#4129=EDGE_CURVE('',#3427,#3426,#2967,.T.);
#4130=EDGE_CURVE('',#3418,#3427,#2113,.T.);
#4131=EDGE_CURVE('',#3428,#3428,#2968,.T.);
#4132=EDGE_CURVE('',#3429,#3419,#2114,.T.);
#4133=EDGE_CURVE('',#3421,#3429,#2115,.T.);
#4134=EDGE_CURVE('',#3417,#3430,#2116,.T.);
#4135=EDGE_CURVE('',#3429,#3430,#2969,.T.);
#4136=EDGE_CURVE('',#3430,#3427,#2117,.T.);
#4137=EDGE_CURVE('',#3431,#3424,#2118,.T.);
#4138=EDGE_CURVE('',#3432,#3431,#2970,.T.);
#4139=EDGE_CURVE('',#3425,#3432,#2119,.T.);
#4140=EDGE_CURVE('',#3433,#3432,#2120,.T.);
#4141=EDGE_CURVE('',#3426,#3433,#2121,.T.);
#4142=EDGE_CURVE('',#3431,#3434,#2122,.T.);
#4143=EDGE_CURVE('',#3433,#3434,#2971,.T.);
#4144=EDGE_CURVE('',#3434,#3423,#2123,.T.);
#4145=EDGE_CURVE('',#3435,#3435,#2972,.T.);
#4146=EDGE_CURVE('',#3436,#3436,#2973,.T.);
#4147=EDGE_CURVE('',#3435,#3422,#2124,.T.);
#4148=EDGE_CURVE('',#3437,#3437,#2974,.T.);
#4149=EDGE_CURVE('',#3438,#3438,#2975,.T.);
#4150=EDGE_CURVE('',#3437,#3436,#2125,.T.);
#4151=EDGE_CURVE('',#3428,#3439,#2126,.T.);
#4152=EDGE_CURVE('',#3439,#3439,#2976,.T.);
#4153=EDGE_CURVE('',#3440,#3440,#2977,.T.);
#4154=EDGE_CURVE('',#3440,#3438,#2127,.T.);
#4155=EDGE_CURVE('',#3441,#3441,#2978,.T.);
#4156=EDGE_CURVE('',#3441,#3442,#2128,.T.);
#4157=EDGE_CURVE('',#3442,#3442,#2979,.T.);
#4158=EDGE_CURVE('',#3443,#3443,#2980,.T.);
#4159=EDGE_CURVE('',#3443,#3444,#2129,.T.);
#4160=EDGE_CURVE('',#3444,#3444,#2981,.T.);
#4161=EDGE_CURVE('',#3445,#3446,#2130,.T.);
#4162=EDGE_CURVE('',#3445,#3446,#2982,.T.);
#4163=EDGE_CURVE('',#3447,#3445,#281,.T.);
#4164=EDGE_CURVE('',#3448,#3447,#2983,.T.);
#4165=EDGE_CURVE('',#3448,#3449,#2131,.T.);
#4166=EDGE_CURVE('',#3450,#3449,#282,.T.);
#4167=EDGE_CURVE('',#3449,#3450,#283,.T.);
#4168=EDGE_CURVE('',#3451,#3448,#2984,.T.);
#4169=EDGE_CURVE('',#3446,#3451,#284,.T.);
#4170=EDGE_CURVE('',#3451,#3447,#2132,.T.);
#4171=EDGE_CURVE('',#3452,#3452,#2985,.T.);
#4172=EDGE_CURVE('',#3452,#3453,#2133,.T.);
#4173=EDGE_CURVE('',#3453,#3453,#2986,.T.);
#4174=EDGE_CURVE('',#3454,#3454,#2987,.T.);
#4175=EDGE_CURVE('',#3454,#3455,#2134,.T.);
#4176=EDGE_CURVE('',#3455,#3455,#2988,.T.);
#4177=EDGE_CURVE('',#3456,#3456,#2989,.T.);
#4178=EDGE_CURVE('',#3456,#3457,#2135,.T.);
#4179=EDGE_CURVE('',#3457,#3457,#2990,.T.);
#4180=EDGE_CURVE('',#3458,#3458,#2991,.T.);
#4181=EDGE_CURVE('',#3458,#3459,#2136,.T.);
#4182=EDGE_CURVE('',#3459,#3459,#2992,.T.);
#4183=EDGE_CURVE('',#3460,#3460,#2993,.T.);
#4184=EDGE_CURVE('',#3461,#3461,#2994,.T.);
#4185=EDGE_CURVE('',#3462,#3462,#2995,.T.);
#4186=EDGE_CURVE('',#3463,#3463,#2996,.T.);
#4187=EDGE_CURVE('',#3460,#3462,#2137,.T.);
#4188=EDGE_CURVE('',#3463,#3464,#2138,.T.);
#4189=EDGE_CURVE('',#3464,#3464,#2997,.T.);
#4190=EDGE_CURVE('',#3465,#3465,#2998,.T.);
#4191=EDGE_CURVE('',#3465,#3461,#2139,.T.);
#4192=EDGE_CURVE('',#3466,#3466,#2999,.T.);
#4193=EDGE_CURVE('',#3466,#3467,#2140,.T.);
#4194=EDGE_CURVE('',#3467,#3467,#3000,.T.);
#4195=EDGE_CURVE('',#3468,#3468,#3001,.T.);
#4196=EDGE_CURVE('',#3468,#3469,#2141,.T.);
#4197=EDGE_CURVE('',#3469,#3469,#3002,.T.);
#4198=EDGE_CURVE('',#3470,#3470,#3003,.T.);
#4199=EDGE_CURVE('',#3470,#3471,#2142,.T.);
#4200=EDGE_CURVE('',#3471,#3471,#3004,.T.);
#4201=EDGE_CURVE('',#3472,#3472,#3005,.T.);
#4202=EDGE_CURVE('',#3472,#3473,#2143,.T.);
#4203=EDGE_CURVE('',#3473,#3473,#3006,.T.);
#4204=EDGE_CURVE('',#3474,#3474,#3007,.T.);
#4205=EDGE_CURVE('',#3474,#3475,#2144,.T.);
#4206=EDGE_CURVE('',#3475,#3475,#3008,.T.);
#4207=EDGE_CURVE('',#3476,#3476,#3009,.T.);
#4208=EDGE_CURVE('',#3476,#3477,#2145,.T.);
#4209=EDGE_CURVE('',#3477,#3477,#3010,.T.);
#4210=EDGE_CURVE('',#3478,#3478,#3011,.T.);
#4211=EDGE_CURVE('',#3478,#3479,#2146,.T.);
#4212=EDGE_CURVE('',#3479,#3479,#3012,.T.);
#4213=EDGE_CURVE('',#3480,#3480,#3013,.T.);
#4214=EDGE_CURVE('',#3480,#3481,#2147,.T.);
#4215=EDGE_CURVE('',#3481,#3481,#3014,.T.);
#4216=EDGE_CURVE('',#3482,#3482,#3015,.T.);
#4217=EDGE_CURVE('',#3483,#3484,#2148,.T.);
#4218=EDGE_CURVE('',#3483,#3485,#2149,.T.);
#4219=EDGE_CURVE('',#3485,#3486,#2150,.T.);
#4220=EDGE_CURVE('',#3484,#3486,#2151,.T.);
#4221=EDGE_CURVE('',#3487,#3483,#2152,.T.);
#4222=EDGE_CURVE('',#3487,#3488,#2153,.T.);
#4223=EDGE_CURVE('',#3488,#3485,#2154,.T.);
#4224=EDGE_CURVE('',#3489,#3487,#2155,.T.);
#4225=EDGE_CURVE('',#3489,#3490,#2156,.T.);
#4226=EDGE_CURVE('',#3490,#3488,#2157,.T.);
#4227=EDGE_CURVE('',#3491,#3489,#2158,.T.);
#4228=EDGE_CURVE('',#3491,#3492,#2159,.T.);
#4229=EDGE_CURVE('',#3492,#3490,#2160,.T.);
#4230=EDGE_CURVE('',#3493,#3491,#2161,.T.);
#4231=EDGE_CURVE('',#3493,#3494,#2162,.T.);
#4232=EDGE_CURVE('',#3494,#3492,#2163,.T.);
#4233=EDGE_CURVE('',#3484,#3493,#2164,.T.);
#4234=EDGE_CURVE('',#3486,#3494,#2165,.T.);
#4235=EDGE_CURVE('',#3495,#3495,#3016,.T.);
#4236=EDGE_CURVE('',#3496,#3496,#3017,.T.);
#4237=EDGE_CURVE('',#3496,#3495,#2166,.T.);
#4238=EDGE_CURVE('',#3482,#3496,#2167,.T.);
#4239=EDGE_CURVE('',#3497,#3498,#2168,.T.);
#4240=EDGE_CURVE('',#3498,#3499,#2169,.T.);
#4241=EDGE_CURVE('',#3499,#3500,#2170,.T.);
#4242=EDGE_CURVE('',#3497,#3500,#2171,.T.);
#4243=EDGE_CURVE('',#3498,#3501,#2172,.T.);
#4244=EDGE_CURVE('',#3501,#3502,#2173,.T.);
#4245=EDGE_CURVE('',#3502,#3499,#2174,.T.);
#4246=EDGE_CURVE('',#3501,#3503,#2175,.T.);
#4247=EDGE_CURVE('',#3503,#3504,#2176,.T.);
#4248=EDGE_CURVE('',#3504,#3502,#2177,.T.);
#4249=EDGE_CURVE('',#3503,#3505,#2178,.T.);
#4250=EDGE_CURVE('',#3505,#3506,#2179,.T.);
#4251=EDGE_CURVE('',#3506,#3504,#2180,.T.);
#4252=EDGE_CURVE('',#3505,#3507,#2181,.T.);
#4253=EDGE_CURVE('',#3507,#3508,#2182,.T.);
#4254=EDGE_CURVE('',#3508,#3506,#2183,.T.);
#4255=EDGE_CURVE('',#3507,#3497,#2184,.T.);
#4256=EDGE_CURVE('',#3500,#3508,#2185,.T.);
#4257=EDGE_CURVE('',#3509,#3509,#3018,.T.);
#4258=EDGE_CURVE('',#3510,#3510,#3019,.T.);
#4259=EDGE_CURVE('',#3511,#3511,#3020,.T.);
#4260=EDGE_CURVE('',#3511,#3510,#2186,.T.);
#4261=EDGE_CURVE('',#3512,#3512,#3021,.T.);
#4262=EDGE_CURVE('',#3512,#3511,#2187,.T.);
#4263=EDGE_CURVE('',#3513,#3513,#3022,.T.);
#4264=EDGE_CURVE('',#3513,#3512,#2188,.T.);
#4265=EDGE_CURVE('',#3514,#3514,#3023,.T.);
#4266=EDGE_CURVE('',#3515,#3515,#3024,.F.);
#4267=EDGE_CURVE('',#3515,#3514,#2189,.T.);
#4268=EDGE_CURVE('',#3509,#3515,#2190,.T.);
#4269=EDGE_CURVE('',#3516,#3516,#3025,.T.);
#4270=EDGE_CURVE('',#3517,#3517,#3026,.T.);
#4271=EDGE_CURVE('',#3517,#3516,#2191,.T.);
#4272=EDGE_CURVE('',#3518,#3518,#3027,.T.);
#4273=EDGE_CURVE('',#3518,#3517,#2192,.T.);
#4274=EDGE_CURVE('',#3519,#3519,#3028,.T.);
#4275=EDGE_CURVE('',#3519,#3518,#2193,.T.);
#4276=EDGE_CURVE('',#3520,#3520,#3029,.T.);
#4277=EDGE_CURVE('',#3521,#3521,#3030,.F.);
#4278=EDGE_CURVE('',#3521,#3520,#2194,.T.);
#4279=EDGE_CURVE('',#3522,#3522,#3031,.F.);
#4280=EDGE_CURVE('',#3522,#3521,#2195,.T.);
#4281=EDGE_CURVE('',#3523,#3523,#3032,.T.);
#4282=EDGE_CURVE('',#3523,#3522,#2196,.T.);
#4283=EDGE_CURVE('',#3524,#3525,#2197,.T.);
#4284=EDGE_CURVE('',#3525,#3526,#2198,.T.);
#4285=EDGE_CURVE('',#3526,#3527,#2199,.T.);
#4286=EDGE_CURVE('',#3524,#3527,#2200,.T.);
#4287=EDGE_CURVE('',#3525,#3528,#2201,.T.);
#4288=EDGE_CURVE('',#3528,#3529,#2202,.T.);
#4289=EDGE_CURVE('',#3529,#3526,#2203,.T.);
#4290=EDGE_CURVE('',#3528,#3530,#2204,.T.);
#4291=EDGE_CURVE('',#3530,#3531,#2205,.T.);
#4292=EDGE_CURVE('',#3531,#3529,#2206,.T.);
#4293=EDGE_CURVE('',#3530,#3532,#2207,.T.);
#4294=EDGE_CURVE('',#3532,#3533,#2208,.T.);
#4295=EDGE_CURVE('',#3533,#3531,#2209,.T.);
#4296=EDGE_CURVE('',#3532,#3534,#2210,.T.);
#4297=EDGE_CURVE('',#3534,#3535,#2211,.T.);
#4298=EDGE_CURVE('',#3535,#3533,#2212,.T.);
#4299=EDGE_CURVE('',#3534,#3524,#2213,.T.);
#4300=EDGE_CURVE('',#3527,#3535,#2214,.T.);
#4301=EDGE_CURVE('',#3536,#3536,#3033,.T.);
#4302=EDGE_CURVE('',#3536,#3537,#2215,.T.);
#4303=EDGE_CURVE('',#3537,#3537,#3034,.T.);
#4304=EDGE_CURVE('',#3538,#3538,#3035,.T.);
#4305=EDGE_CURVE('',#3538,#3539,#2216,.T.);
#4306=EDGE_CURVE('',#3539,#3539,#3036,.T.);
#4307=EDGE_CURVE('',#3540,#3541,#2217,.T.);
#4308=EDGE_CURVE('',#3542,#3540,#3037,.T.);
#4309=EDGE_CURVE('',#3543,#3542,#2218,.T.);
#4310=EDGE_CURVE('',#3543,#3541,#3038,.T.);
#4311=EDGE_CURVE('',#3541,#3544,#2219,.T.);
#4312=EDGE_CURVE('',#3545,#3544,#2220,.T.);
#4313=EDGE_CURVE('',#3540,#3545,#2221,.T.);
#4314=EDGE_CURVE('',#3546,#3543,#2222,.T.);
#4315=EDGE_CURVE('',#3544,#3546,#3039,.T.);
#4316=EDGE_CURVE('',#3547,#3542,#2223,.T.);
#4317=EDGE_CURVE('',#3546,#3547,#2224,.T.);
#4318=EDGE_CURVE('',#3545,#3547,#3040,.T.);
#4319=EDGE_CURVE('',#3548,#3548,#3041,.T.);
#4320=EDGE_CURVE('',#3548,#3549,#2225,.T.);
#4321=EDGE_CURVE('',#3549,#3549,#3042,.T.);
#4322=EDGE_CURVE('',#3550,#3550,#3043,.T.);
#4323=EDGE_CURVE('',#3550,#3551,#2226,.T.);
#4324=EDGE_CURVE('',#3551,#3551,#3044,.T.);
#4325=EDGE_CURVE('',#3552,#3552,#3045,.T.);
#4326=EDGE_CURVE('',#3552,#3553,#2227,.T.);
#4327=EDGE_CURVE('',#3553,#3553,#3046,.T.);
#4328=EDGE_CURVE('',#3554,#3554,#3047,.T.);
#4329=EDGE_CURVE('',#3554,#3555,#2228,.T.);
#4330=EDGE_CURVE('',#3555,#3555,#3048,.T.);
#4331=EDGE_CURVE('',#3556,#3556,#3049,.T.);
#4332=EDGE_CURVE('',#3556,#3557,#2229,.T.);
#4333=EDGE_CURVE('',#3557,#3557,#3050,.T.);
#4334=EDGE_CURVE('',#3558,#3559,#2230,.T.);
#4335=EDGE_CURVE('',#3560,#3558,#2231,.T.);
#4336=EDGE_CURVE('',#3561,#3560,#2232,.T.);
#4337=EDGE_CURVE('',#3559,#3561,#2233,.T.);
#4338=EDGE_CURVE('',#3560,#3562,#2234,.T.);
#4339=EDGE_CURVE('',#3563,#3562,#2235,.T.);
#4340=EDGE_CURVE('',#3564,#3563,#2236,.T.);
#4341=EDGE_CURVE('',#3564,#3565,#2237,.T.);
#4342=EDGE_CURVE('',#3561,#3565,#2238,.T.);
#4343=EDGE_CURVE('',#3566,#3558,#2239,.T.);
#4344=EDGE_CURVE('',#3562,#3566,#3051,.T.);
#4345=EDGE_CURVE('',#3567,#3559,#2240,.T.);
#4346=EDGE_CURVE('',#3568,#3567,#2241,.T.);
#4347=EDGE_CURVE('',#3569,#3568,#2242,.T.);
#4348=EDGE_CURVE('',#3566,#3569,#2243,.T.);
#4349=EDGE_CURVE('',#3570,#3571,#2244,.T.);
#4350=EDGE_CURVE('',#3565,#3570,#2245,.T.);
#4351=EDGE_CURVE('',#3571,#3564,#2246,.T.);
#4352=EDGE_CURVE('',#3568,#3572,#2247,.T.);
#4353=EDGE_CURVE('',#3573,#3567,#2248,.T.);
#4354=EDGE_CURVE('',#3572,#3573,#2249,.T.);
#4355=EDGE_CURVE('',#3573,#3570,#3052,.T.);
#4356=EDGE_CURVE('',#3574,#3574,#3053,.T.);
#4357=EDGE_CURVE('',#3574,#3573,#2250,.T.);
#4358=EDGE_CURVE('',#3571,#3572,#3054,.T.);
#4359=EDGE_CURVE('',#3563,#3575,#3055,.T.);
#4360=EDGE_CURVE('',#3575,#3569,#3056,.T.);
#4361=EDGE_CURVE('',#3575,#3576,#2251,.T.);
#4362=EDGE_CURVE('',#3576,#3576,#3057,.T.);
#4363=EDGE_CURVE('',#3577,#3578,#2252,.T.);
#4364=EDGE_CURVE('',#3577,#3578,#3058,.T.);
#4365=EDGE_CURVE('',#3579,#3577,#285,.T.);
#4366=EDGE_CURVE('',#3580,#3579,#3059,.T.);
#4367=EDGE_CURVE('',#3580,#3581,#2253,.T.);
#4368=EDGE_CURVE('',#3581,#3581,#3060,.T.);
#4369=EDGE_CURVE('',#3582,#3580,#3061,.T.);
#4370=EDGE_CURVE('',#3578,#3582,#286,.T.);
#4371=EDGE_CURVE('',#3582,#3579,#2254,.T.);
#4372=EDGE_CURVE('',#3583,#3583,#3062,.T.);
#4373=EDGE_CURVE('',#3583,#3584,#2255,.T.);
#4374=EDGE_CURVE('',#3584,#3584,#3063,.T.);
#4375=EDGE_CURVE('',#3585,#3586,#2256,.T.);
#4376=EDGE_CURVE('',#3586,#3587,#2257,.T.);
#4377=EDGE_CURVE('',#3588,#3587,#2258,.T.);
#4378=EDGE_CURVE('',#3585,#3588,#2259,.T.);
#4379=EDGE_CURVE('',#3589,#3590,#2260,.T.);
#4380=EDGE_CURVE('',#3590,#3585,#2261,.T.);
#4381=EDGE_CURVE('',#3589,#3588,#2262,.T.);
#4382=EDGE_CURVE('',#3591,#3589,#2263,.T.);
#4383=EDGE_CURVE('',#3587,#3591,#2264,.T.);
#4384=EDGE_CURVE('',#3590,#3592,#2265,.T.);
#4385=EDGE_CURVE('',#3586,#3592,#2266,.T.);
#4386=EDGE_CURVE('',#3592,#3591,#2267,.T.);
#4387=EDGE_CURVE('',#3593,#3593,#3064,.T.);
#4388=EDGE_CURVE('',#3594,#3594,#3065,.T.);
#4389=EDGE_CURVE('',#3593,#3595,#2268,.T.);
#4390=EDGE_CURVE('',#3595,#3595,#3066,.T.);
#4391=EDGE_CURVE('',#3596,#3596,#3067,.T.);
#4392=EDGE_CURVE('',#3596,#3594,#2269,.T.);
#4393=EDGE_CURVE('',#3597,#3597,#3068,.T.);
#4394=EDGE_CURVE('',#3597,#3598,#2270,.T.);
#4395=EDGE_CURVE('',#3598,#3598,#3069,.T.);
#4396=EDGE_CURVE('',#3599,#3600,#2271,.T.);
#4397=EDGE_CURVE('',#3599,#3601,#2272,.T.);
#4398=EDGE_CURVE('',#3601,#3602,#2273,.T.);
#4399=EDGE_CURVE('',#3600,#3602,#2274,.T.);
#4400=EDGE_CURVE('',#3603,#3599,#2275,.T.);
#4401=EDGE_CURVE('',#3603,#3604,#2276,.T.);
#4402=EDGE_CURVE('',#3604,#3601,#2277,.T.);
#4403=EDGE_CURVE('',#3605,#3603,#2278,.T.);
#4404=EDGE_CURVE('',#3605,#3606,#2279,.T.);
#4405=EDGE_CURVE('',#3606,#3604,#2280,.T.);
#4406=EDGE_CURVE('',#3607,#3605,#2281,.T.);
#4407=EDGE_CURVE('',#3607,#3608,#2282,.T.);
#4408=EDGE_CURVE('',#3608,#3606,#2283,.T.);
#4409=EDGE_CURVE('',#3609,#3607,#2284,.T.);
#4410=EDGE_CURVE('',#3609,#3610,#2285,.T.);
#4411=EDGE_CURVE('',#3610,#3608,#2286,.T.);
#4412=EDGE_CURVE('',#3600,#3609,#2287,.T.);
#4413=EDGE_CURVE('',#3602,#3610,#2288,.T.);
#4414=EDGE_CURVE('',#3611,#3611,#3070,.T.);
#4415=EDGE_CURVE('',#3612,#3612,#3071,.T.);
#4416=EDGE_CURVE('',#3612,#3611,#2289,.T.);
#4417=EDGE_CURVE('',#3613,#3613,#3072,.F.);
#4418=EDGE_CURVE('',#3613,#3612,#2290,.T.);
#4419=EDGE_CURVE('',#3614,#3614,#3073,.T.);
#4420=EDGE_CURVE('',#3614,#3613,#2291,.T.);
#4421=ORIENTED_EDGE('',*,*,#3615,.F.);
#4422=ORIENTED_EDGE('',*,*,#3616,.T.);
#4423=ORIENTED_EDGE('',*,*,#3617,.F.);
#4424=ORIENTED_EDGE('',*,*,#3616,.F.);
#4425=ORIENTED_EDGE('',*,*,#3618,.F.);
#4426=ORIENTED_EDGE('',*,*,#3619,.T.);
#4427=ORIENTED_EDGE('',*,*,#3620,.F.);
#4428=ORIENTED_EDGE('',*,*,#3619,.F.);
#4429=ORIENTED_EDGE('',*,*,#3621,.F.);
#4430=ORIENTED_EDGE('',*,*,#3622,.T.);
#4431=ORIENTED_EDGE('',*,*,#3623,.F.);
#4432=ORIENTED_EDGE('',*,*,#3622,.F.);
#4433=ORIENTED_EDGE('',*,*,#3624,.F.);
#4434=ORIENTED_EDGE('',*,*,#3625,.T.);
#4435=ORIENTED_EDGE('',*,*,#3626,.F.);
#4436=ORIENTED_EDGE('',*,*,#3625,.F.);
#4437=ORIENTED_EDGE('',*,*,#3627,.F.);
#4438=ORIENTED_EDGE('',*,*,#3628,.T.);
#4439=ORIENTED_EDGE('',*,*,#3629,.F.);
#4440=ORIENTED_EDGE('',*,*,#3628,.F.);
#4441=ORIENTED_EDGE('',*,*,#3630,.F.);
#4442=ORIENTED_EDGE('',*,*,#3631,.T.);
#4443=ORIENTED_EDGE('',*,*,#3632,.F.);
#4444=ORIENTED_EDGE('',*,*,#3631,.F.);
#4445=ORIENTED_EDGE('',*,*,#3633,.F.);
#4446=ORIENTED_EDGE('',*,*,#3634,.T.);
#4447=ORIENTED_EDGE('',*,*,#3635,.F.);
#4448=ORIENTED_EDGE('',*,*,#3634,.F.);
#4449=ORIENTED_EDGE('',*,*,#3636,.F.);
#4450=ORIENTED_EDGE('',*,*,#3637,.T.);
#4451=ORIENTED_EDGE('',*,*,#3638,.F.);
#4452=ORIENTED_EDGE('',*,*,#3637,.F.);
#4453=ORIENTED_EDGE('',*,*,#3639,.T.);
#4454=ORIENTED_EDGE('',*,*,#3640,.T.);
#4455=ORIENTED_EDGE('',*,*,#3641,.F.);
#4456=ORIENTED_EDGE('',*,*,#3642,.F.);
#4457=ORIENTED_EDGE('',*,*,#3643,.T.);
#4458=ORIENTED_EDGE('',*,*,#3642,.T.);
#4459=ORIENTED_EDGE('',*,*,#3644,.F.);
#4460=ORIENTED_EDGE('',*,*,#3645,.F.);
#4461=ORIENTED_EDGE('',*,*,#3646,.T.);
#4462=ORIENTED_EDGE('',*,*,#3645,.T.);
#4463=ORIENTED_EDGE('',*,*,#3647,.F.);
#4464=ORIENTED_EDGE('',*,*,#3648,.F.);
#4465=ORIENTED_EDGE('',*,*,#3649,.T.);
#4466=ORIENTED_EDGE('',*,*,#3648,.T.);
#4467=ORIENTED_EDGE('',*,*,#3650,.F.);
#4468=ORIENTED_EDGE('',*,*,#3640,.F.);
#4469=ORIENTED_EDGE('',*,*,#3650,.T.);
#4470=ORIENTED_EDGE('',*,*,#3647,.T.);
#4471=ORIENTED_EDGE('',*,*,#3644,.T.);
#4472=ORIENTED_EDGE('',*,*,#3641,.T.);
#4473=ORIENTED_EDGE('',*,*,#3638,.T.);
#4474=ORIENTED_EDGE('',*,*,#3635,.T.);
#4475=ORIENTED_EDGE('',*,*,#3632,.T.);
#4476=ORIENTED_EDGE('',*,*,#3629,.T.);
#4477=ORIENTED_EDGE('',*,*,#3626,.T.);
#4478=ORIENTED_EDGE('',*,*,#3623,.T.);
#4479=ORIENTED_EDGE('',*,*,#3620,.T.);
#4480=ORIENTED_EDGE('',*,*,#3617,.T.);
#4481=ORIENTED_EDGE('',*,*,#3649,.F.);
#4482=ORIENTED_EDGE('',*,*,#3639,.F.);
#4483=ORIENTED_EDGE('',*,*,#3643,.F.);
#4484=ORIENTED_EDGE('',*,*,#3646,.F.);
#4485=ORIENTED_EDGE('',*,*,#3636,.T.);
#4486=ORIENTED_EDGE('',*,*,#3633,.T.);
#4487=ORIENTED_EDGE('',*,*,#3630,.T.);
#4488=ORIENTED_EDGE('',*,*,#3627,.T.);
#4489=ORIENTED_EDGE('',*,*,#3624,.T.);
#4490=ORIENTED_EDGE('',*,*,#3621,.T.);
#4491=ORIENTED_EDGE('',*,*,#3618,.T.);
#4492=ORIENTED_EDGE('',*,*,#3615,.T.);
#4493=ORIENTED_EDGE('',*,*,#3651,.T.);
#4494=ORIENTED_EDGE('',*,*,#3652,.T.);
#4495=ORIENTED_EDGE('',*,*,#3653,.F.);
#4496=ORIENTED_EDGE('',*,*,#3654,.F.);
#4497=ORIENTED_EDGE('',*,*,#3655,.T.);
#4498=ORIENTED_EDGE('',*,*,#3654,.T.);
#4499=ORIENTED_EDGE('',*,*,#3656,.F.);
#4500=ORIENTED_EDGE('',*,*,#3657,.F.);
#4501=ORIENTED_EDGE('',*,*,#3658,.T.);
#4502=ORIENTED_EDGE('',*,*,#3657,.T.);
#4503=ORIENTED_EDGE('',*,*,#3659,.F.);
#4504=ORIENTED_EDGE('',*,*,#3660,.F.);
#4505=ORIENTED_EDGE('',*,*,#3661,.T.);
#4506=ORIENTED_EDGE('',*,*,#3660,.T.);
#4507=ORIENTED_EDGE('',*,*,#3662,.F.);
#4508=ORIENTED_EDGE('',*,*,#3652,.F.);
#4509=ORIENTED_EDGE('',*,*,#3662,.T.);
#4510=ORIENTED_EDGE('',*,*,#3659,.T.);
#4511=ORIENTED_EDGE('',*,*,#3656,.T.);
#4512=ORIENTED_EDGE('',*,*,#3653,.T.);
#4513=ORIENTED_EDGE('',*,*,#3661,.F.);
#4514=ORIENTED_EDGE('',*,*,#3651,.F.);
#4515=ORIENTED_EDGE('',*,*,#3655,.F.);
#4516=ORIENTED_EDGE('',*,*,#3658,.F.);
#4517=ORIENTED_EDGE('',*,*,#3663,.T.);
#4518=ORIENTED_EDGE('',*,*,#3664,.T.);
#4519=ORIENTED_EDGE('',*,*,#3665,.F.);
#4520=ORIENTED_EDGE('',*,*,#3666,.F.);
#4521=ORIENTED_EDGE('',*,*,#3667,.T.);
#4522=ORIENTED_EDGE('',*,*,#3666,.T.);
#4523=ORIENTED_EDGE('',*,*,#3668,.F.);
#4524=ORIENTED_EDGE('',*,*,#3669,.F.);
#4525=ORIENTED_EDGE('',*,*,#3670,.T.);
#4526=ORIENTED_EDGE('',*,*,#3669,.T.);
#4527=ORIENTED_EDGE('',*,*,#3671,.F.);
#4528=ORIENTED_EDGE('',*,*,#3672,.F.);
#4529=ORIENTED_EDGE('',*,*,#3673,.T.);
#4530=ORIENTED_EDGE('',*,*,#3672,.T.);
#4531=ORIENTED_EDGE('',*,*,#3674,.F.);
#4532=ORIENTED_EDGE('',*,*,#3664,.F.);
#4533=ORIENTED_EDGE('',*,*,#3674,.T.);
#4534=ORIENTED_EDGE('',*,*,#3671,.T.);
#4535=ORIENTED_EDGE('',*,*,#3668,.T.);
#4536=ORIENTED_EDGE('',*,*,#3665,.T.);
#4537=ORIENTED_EDGE('',*,*,#3673,.F.);
#4538=ORIENTED_EDGE('',*,*,#3663,.F.);
#4539=ORIENTED_EDGE('',*,*,#3667,.F.);
#4540=ORIENTED_EDGE('',*,*,#3670,.F.);
#4541=ORIENTED_EDGE('',*,*,#3675,.F.);
#4542=ORIENTED_EDGE('',*,*,#3676,.T.);
#4543=ORIENTED_EDGE('',*,*,#3677,.F.);
#4544=ORIENTED_EDGE('',*,*,#3676,.F.);
#4545=ORIENTED_EDGE('',*,*,#3678,.F.);
#4546=ORIENTED_EDGE('',*,*,#3679,.T.);
#4547=ORIENTED_EDGE('',*,*,#3680,.F.);
#4548=ORIENTED_EDGE('',*,*,#3679,.F.);
#4549=ORIENTED_EDGE('',*,*,#3678,.T.);
#4550=ORIENTED_EDGE('',*,*,#3681,.F.);
#4551=ORIENTED_EDGE('',*,*,#3682,.T.);
#4552=ORIENTED_EDGE('',*,*,#3683,.F.);
#4553=ORIENTED_EDGE('',*,*,#3682,.F.);
#4554=ORIENTED_EDGE('',*,*,#3681,.T.);
#4555=ORIENTED_EDGE('',*,*,#3684,.F.);
#4556=ORIENTED_EDGE('',*,*,#3685,.T.);
#4557=ORIENTED_EDGE('',*,*,#3686,.F.);
#4558=ORIENTED_EDGE('',*,*,#3685,.F.);
#4559=ORIENTED_EDGE('',*,*,#3684,.T.);
#4560=ORIENTED_EDGE('',*,*,#3687,.F.);
#4561=ORIENTED_EDGE('',*,*,#3688,.T.);
#4562=ORIENTED_EDGE('',*,*,#3689,.F.);
#4563=ORIENTED_EDGE('',*,*,#3688,.F.);
#4564=ORIENTED_EDGE('',*,*,#3687,.T.);
#4565=ORIENTED_EDGE('',*,*,#3690,.F.);
#4566=ORIENTED_EDGE('',*,*,#3691,.T.);
#4567=ORIENTED_EDGE('',*,*,#3692,.F.);
#4568=ORIENTED_EDGE('',*,*,#3691,.F.);
#4569=ORIENTED_EDGE('',*,*,#3693,.F.);
#4570=ORIENTED_EDGE('',*,*,#3694,.T.);
#4571=ORIENTED_EDGE('',*,*,#3695,.F.);
#4572=ORIENTED_EDGE('',*,*,#3694,.F.);
#4573=ORIENTED_EDGE('',*,*,#3696,.F.);
#4574=ORIENTED_EDGE('',*,*,#3697,.T.);
#4575=ORIENTED_EDGE('',*,*,#3698,.F.);
#4576=ORIENTED_EDGE('',*,*,#3697,.F.);
#4577=ORIENTED_EDGE('',*,*,#3699,.F.);
#4578=ORIENTED_EDGE('',*,*,#3700,.T.);
#4579=ORIENTED_EDGE('',*,*,#3701,.F.);
#4580=ORIENTED_EDGE('',*,*,#3700,.F.);
#4581=ORIENTED_EDGE('',*,*,#3702,.F.);
#4582=ORIENTED_EDGE('',*,*,#3703,.T.);
#4583=ORIENTED_EDGE('',*,*,#3704,.F.);
#4584=ORIENTED_EDGE('',*,*,#3703,.F.);
#4585=ORIENTED_EDGE('',*,*,#3705,.F.);
#4586=ORIENTED_EDGE('',*,*,#3706,.T.);
#4587=ORIENTED_EDGE('',*,*,#3707,.F.);
#4588=ORIENTED_EDGE('',*,*,#3706,.F.);
#4589=ORIENTED_EDGE('',*,*,#3708,.F.);
#4590=ORIENTED_EDGE('',*,*,#3709,.T.);
#4591=ORIENTED_EDGE('',*,*,#3710,.F.);
#4592=ORIENTED_EDGE('',*,*,#3709,.F.);
#4593=ORIENTED_EDGE('',*,*,#3711,.F.);
#4594=ORIENTED_EDGE('',*,*,#3712,.T.);
#4595=ORIENTED_EDGE('',*,*,#3713,.F.);
#4596=ORIENTED_EDGE('',*,*,#3712,.F.);
#4597=ORIENTED_EDGE('',*,*,#3714,.F.);
#4598=ORIENTED_EDGE('',*,*,#3715,.T.);
#4599=ORIENTED_EDGE('',*,*,#3716,.F.);
#4600=ORIENTED_EDGE('',*,*,#3715,.F.);
#4601=ORIENTED_EDGE('',*,*,#3714,.T.);
#4602=ORIENTED_EDGE('',*,*,#3717,.F.);
#4603=ORIENTED_EDGE('',*,*,#3718,.F.);
#4604=ORIENTED_EDGE('',*,*,#3719,.T.);
#4605=ORIENTED_EDGE('',*,*,#3717,.T.);
#4606=ORIENTED_EDGE('',*,*,#3719,.F.);
#4607=ORIENTED_EDGE('',*,*,#3720,.F.);
#4608=ORIENTED_EDGE('',*,*,#3721,.T.);
#4609=ORIENTED_EDGE('',*,*,#3722,.F.);
#4610=ORIENTED_EDGE('',*,*,#3721,.F.);
#4611=ORIENTED_EDGE('',*,*,#3723,.F.);
#4612=ORIENTED_EDGE('',*,*,#3724,.T.);
#4613=ORIENTED_EDGE('',*,*,#3725,.F.);
#4614=ORIENTED_EDGE('',*,*,#3726,.F.);
#4615=ORIENTED_EDGE('',*,*,#3723,.T.);
#4616=ORIENTED_EDGE('',*,*,#3727,.T.);
#4617=ORIENTED_EDGE('',*,*,#3728,.T.);
#4618=ORIENTED_EDGE('',*,*,#3729,.F.);
#4619=ORIENTED_EDGE('',*,*,#3730,.F.);
#4620=ORIENTED_EDGE('',*,*,#3731,.T.);
#4621=ORIENTED_EDGE('',*,*,#3732,.T.);
#4622=ORIENTED_EDGE('',*,*,#3733,.T.);
#4623=ORIENTED_EDGE('',*,*,#3734,.F.);
#4624=ORIENTED_EDGE('',*,*,#3735,.T.);
#4625=ORIENTED_EDGE('',*,*,#3675,.T.);
#4626=ORIENTED_EDGE('',*,*,#3720,.T.);
#4627=ORIENTED_EDGE('',*,*,#3699,.T.);
#4628=ORIENTED_EDGE('',*,*,#3696,.T.);
#4629=ORIENTED_EDGE('',*,*,#3693,.T.);
#4630=ORIENTED_EDGE('',*,*,#3690,.T.);
#4631=ORIENTED_EDGE('',*,*,#3726,.T.);
#4632=ORIENTED_EDGE('',*,*,#3736,.F.);
#4633=ORIENTED_EDGE('',*,*,#3737,.F.);
#4634=ORIENTED_EDGE('',*,*,#3727,.F.);
#4635=ORIENTED_EDGE('',*,*,#3716,.T.);
#4636=ORIENTED_EDGE('',*,*,#3689,.T.);
#4637=ORIENTED_EDGE('',*,*,#3686,.T.);
#4638=ORIENTED_EDGE('',*,*,#3683,.T.);
#4639=ORIENTED_EDGE('',*,*,#3680,.T.);
#4640=ORIENTED_EDGE('',*,*,#3738,.T.);
#4641=ORIENTED_EDGE('',*,*,#3739,.T.);
#4642=ORIENTED_EDGE('',*,*,#3740,.T.);
#4643=ORIENTED_EDGE('',*,*,#3741,.T.);
#4644=ORIENTED_EDGE('',*,*,#3742,.F.);
#4645=ORIENTED_EDGE('',*,*,#3743,.F.);
#4646=ORIENTED_EDGE('',*,*,#3731,.F.);
#4647=ORIENTED_EDGE('',*,*,#3744,.F.);
#4648=ORIENTED_EDGE('',*,*,#3713,.T.);
#4649=ORIENTED_EDGE('',*,*,#3710,.T.);
#4650=ORIENTED_EDGE('',*,*,#3707,.T.);
#4651=ORIENTED_EDGE('',*,*,#3704,.T.);
#4652=ORIENTED_EDGE('',*,*,#3745,.T.);
#4653=ORIENTED_EDGE('',*,*,#3746,.T.);
#4654=ORIENTED_EDGE('',*,*,#3741,.F.);
#4655=ORIENTED_EDGE('',*,*,#3747,.F.);
#4656=ORIENTED_EDGE('',*,*,#3748,.T.);
#4657=ORIENTED_EDGE('',*,*,#3747,.T.);
#4658=ORIENTED_EDGE('',*,*,#3740,.F.);
#4659=ORIENTED_EDGE('',*,*,#3749,.F.);
#4660=ORIENTED_EDGE('',*,*,#3750,.T.);
#4661=ORIENTED_EDGE('',*,*,#3749,.T.);
#4662=ORIENTED_EDGE('',*,*,#3739,.F.);
#4663=ORIENTED_EDGE('',*,*,#3751,.F.);
#4664=ORIENTED_EDGE('',*,*,#3752,.T.);
#4665=ORIENTED_EDGE('',*,*,#3751,.T.);
#4666=ORIENTED_EDGE('',*,*,#3738,.F.);
#4667=ORIENTED_EDGE('',*,*,#3746,.F.);
#4668=ORIENTED_EDGE('',*,*,#3743,.T.);
#4669=ORIENTED_EDGE('',*,*,#3753,.T.);
#4670=ORIENTED_EDGE('',*,*,#3754,.T.);
#4671=ORIENTED_EDGE('',*,*,#3732,.F.);
#4672=ORIENTED_EDGE('',*,*,#3755,.F.);
#4673=ORIENTED_EDGE('',*,*,#3734,.T.);
#4674=ORIENTED_EDGE('',*,*,#3756,.F.);
#4675=ORIENTED_EDGE('',*,*,#3757,.F.);
#4676=ORIENTED_EDGE('',*,*,#3725,.T.);
#4677=ORIENTED_EDGE('',*,*,#3758,.T.);
#4678=ORIENTED_EDGE('',*,*,#3757,.T.);
#4679=ORIENTED_EDGE('',*,*,#3759,.T.);
#4680=ORIENTED_EDGE('',*,*,#3753,.F.);
#4681=ORIENTED_EDGE('',*,*,#3742,.T.);
#4682=ORIENTED_EDGE('',*,*,#3760,.T.);
#4683=ORIENTED_EDGE('',*,*,#3761,.F.);
#4684=ORIENTED_EDGE('',*,*,#3762,.F.);
#4685=ORIENTED_EDGE('',*,*,#3736,.T.);
#4686=ORIENTED_EDGE('',*,*,#3677,.T.);
#4687=ORIENTED_EDGE('',*,*,#3722,.T.);
#4688=ORIENTED_EDGE('',*,*,#3701,.T.);
#4689=ORIENTED_EDGE('',*,*,#3698,.T.);
#4690=ORIENTED_EDGE('',*,*,#3695,.T.);
#4691=ORIENTED_EDGE('',*,*,#3692,.T.);
#4692=ORIENTED_EDGE('',*,*,#3756,.T.);
#4693=ORIENTED_EDGE('',*,*,#3733,.F.);
#4694=ORIENTED_EDGE('',*,*,#3754,.F.);
#4695=ORIENTED_EDGE('',*,*,#3759,.F.);
#4696=ORIENTED_EDGE('',*,*,#3735,.F.);
#4697=ORIENTED_EDGE('',*,*,#3755,.T.);
#4698=ORIENTED_EDGE('',*,*,#3758,.F.);
#4699=ORIENTED_EDGE('',*,*,#3724,.F.);
#4700=ORIENTED_EDGE('',*,*,#3718,.T.);
#4701=ORIENTED_EDGE('',*,*,#3737,.T.);
#4702=ORIENTED_EDGE('',*,*,#3762,.T.);
#4703=ORIENTED_EDGE('',*,*,#3763,.F.);
#4704=ORIENTED_EDGE('',*,*,#3728,.F.);
#4705=ORIENTED_EDGE('',*,*,#3744,.T.);
#4706=ORIENTED_EDGE('',*,*,#3730,.T.);
#4707=ORIENTED_EDGE('',*,*,#3764,.F.);
#4708=ORIENTED_EDGE('',*,*,#3760,.F.);
#4709=ORIENTED_EDGE('',*,*,#3764,.T.);
#4710=ORIENTED_EDGE('',*,*,#3729,.T.);
#4711=ORIENTED_EDGE('',*,*,#3763,.T.);
#4712=ORIENTED_EDGE('',*,*,#3761,.T.);
#4713=ORIENTED_EDGE('',*,*,#3752,.F.);
#4714=ORIENTED_EDGE('',*,*,#3745,.F.);
#4715=ORIENTED_EDGE('',*,*,#3748,.F.);
#4716=ORIENTED_EDGE('',*,*,#3750,.F.);
#4717=ORIENTED_EDGE('',*,*,#3702,.T.);
#4718=ORIENTED_EDGE('',*,*,#3705,.T.);
#4719=ORIENTED_EDGE('',*,*,#3708,.T.);
#4720=ORIENTED_EDGE('',*,*,#3711,.T.);
#4721=ORIENTED_EDGE('',*,*,#3765,.F.);
#4722=ORIENTED_EDGE('',*,*,#3766,.T.);
#4723=ORIENTED_EDGE('',*,*,#3767,.F.);
#4724=ORIENTED_EDGE('',*,*,#3766,.F.);
#4725=ORIENTED_EDGE('',*,*,#3768,.F.);
#4726=ORIENTED_EDGE('',*,*,#3769,.T.);
#4727=ORIENTED_EDGE('',*,*,#3770,.F.);
#4728=ORIENTED_EDGE('',*,*,#3769,.F.);
#4729=ORIENTED_EDGE('',*,*,#3771,.F.);
#4730=ORIENTED_EDGE('',*,*,#3772,.T.);
#4731=ORIENTED_EDGE('',*,*,#3773,.F.);
#4732=ORIENTED_EDGE('',*,*,#3772,.F.);
#4733=ORIENTED_EDGE('',*,*,#3774,.F.);
#4734=ORIENTED_EDGE('',*,*,#3775,.T.);
#4735=ORIENTED_EDGE('',*,*,#3776,.F.);
#4736=ORIENTED_EDGE('',*,*,#3775,.F.);
#4737=ORIENTED_EDGE('',*,*,#3777,.F.);
#4738=ORIENTED_EDGE('',*,*,#3778,.T.);
#4739=ORIENTED_EDGE('',*,*,#3779,.F.);
#4740=ORIENTED_EDGE('',*,*,#3778,.F.);
#4741=ORIENTED_EDGE('',*,*,#3777,.T.);
#4742=ORIENTED_EDGE('',*,*,#3780,.T.);
#4743=ORIENTED_EDGE('',*,*,#3780,.F.);
#4744=ORIENTED_EDGE('',*,*,#3781,.T.);
#4745=ORIENTED_EDGE('',*,*,#3782,.T.);
#4746=ORIENTED_EDGE('',*,*,#3781,.F.);
#4747=ORIENTED_EDGE('',*,*,#3783,.F.);
#4748=ORIENTED_EDGE('',*,*,#3784,.T.);
#4749=ORIENTED_EDGE('',*,*,#3785,.T.);
#4750=ORIENTED_EDGE('',*,*,#3784,.F.);
#4751=ORIENTED_EDGE('',*,*,#3783,.T.);
#4752=ORIENTED_EDGE('',*,*,#3779,.T.);
#4753=ORIENTED_EDGE('',*,*,#3776,.T.);
#4754=ORIENTED_EDGE('',*,*,#3773,.T.);
#4755=ORIENTED_EDGE('',*,*,#3770,.T.);
#4756=ORIENTED_EDGE('',*,*,#3767,.T.);
#4757=ORIENTED_EDGE('',*,*,#3785,.F.);
#4758=ORIENTED_EDGE('',*,*,#3782,.F.);
#4759=ORIENTED_EDGE('',*,*,#3774,.T.);
#4760=ORIENTED_EDGE('',*,*,#3771,.T.);
#4761=ORIENTED_EDGE('',*,*,#3768,.T.);
#4762=ORIENTED_EDGE('',*,*,#3765,.T.);
#4763=ORIENTED_EDGE('',*,*,#3786,.F.);
#4764=ORIENTED_EDGE('',*,*,#3787,.T.);
#4765=ORIENTED_EDGE('',*,*,#3788,.F.);
#4766=ORIENTED_EDGE('',*,*,#3787,.F.);
#4767=ORIENTED_EDGE('',*,*,#3789,.F.);
#4768=ORIENTED_EDGE('',*,*,#3790,.T.);
#4769=ORIENTED_EDGE('',*,*,#3791,.F.);
#4770=ORIENTED_EDGE('',*,*,#3790,.F.);
#4771=ORIENTED_EDGE('',*,*,#3792,.F.);
#4772=ORIENTED_EDGE('',*,*,#3793,.T.);
#4773=ORIENTED_EDGE('',*,*,#3794,.F.);
#4774=ORIENTED_EDGE('',*,*,#3793,.F.);
#4775=ORIENTED_EDGE('',*,*,#3795,.F.);
#4776=ORIENTED_EDGE('',*,*,#3796,.T.);
#4777=ORIENTED_EDGE('',*,*,#3797,.F.);
#4778=ORIENTED_EDGE('',*,*,#3796,.F.);
#4779=ORIENTED_EDGE('',*,*,#3798,.F.);
#4780=ORIENTED_EDGE('',*,*,#3799,.T.);
#4781=ORIENTED_EDGE('',*,*,#3800,.T.);
#4782=ORIENTED_EDGE('',*,*,#3799,.F.);
#4783=ORIENTED_EDGE('',*,*,#3800,.F.);
#4784=ORIENTED_EDGE('',*,*,#3801,.F.);
#4785=ORIENTED_EDGE('',*,*,#3802,.F.);
#4786=ORIENTED_EDGE('',*,*,#3803,.T.);
#4787=ORIENTED_EDGE('',*,*,#3801,.T.);
#4788=ORIENTED_EDGE('',*,*,#3803,.F.);
#4789=ORIENTED_EDGE('',*,*,#3804,.F.);
#4790=ORIENTED_EDGE('',*,*,#3805,.T.);
#4791=ORIENTED_EDGE('',*,*,#3806,.T.);
#4792=ORIENTED_EDGE('',*,*,#3805,.F.);
#4793=ORIENTED_EDGE('',*,*,#3804,.T.);
#4794=ORIENTED_EDGE('',*,*,#3802,.T.);
#4795=ORIENTED_EDGE('',*,*,#3797,.T.);
#4796=ORIENTED_EDGE('',*,*,#3794,.T.);
#4797=ORIENTED_EDGE('',*,*,#3791,.T.);
#4798=ORIENTED_EDGE('',*,*,#3788,.T.);
#4799=ORIENTED_EDGE('',*,*,#3806,.F.);
#4800=ORIENTED_EDGE('',*,*,#3798,.T.);
#4801=ORIENTED_EDGE('',*,*,#3795,.T.);
#4802=ORIENTED_EDGE('',*,*,#3792,.T.);
#4803=ORIENTED_EDGE('',*,*,#3789,.T.);
#4804=ORIENTED_EDGE('',*,*,#3786,.T.);
#4805=ORIENTED_EDGE('',*,*,#3807,.F.);
#4806=ORIENTED_EDGE('',*,*,#3808,.T.);
#4807=ORIENTED_EDGE('',*,*,#3809,.F.);
#4808=ORIENTED_EDGE('',*,*,#3808,.F.);
#4809=ORIENTED_EDGE('',*,*,#3807,.T.);
#4810=ORIENTED_EDGE('',*,*,#3810,.F.);
#4811=ORIENTED_EDGE('',*,*,#3811,.F.);
#4812=ORIENTED_EDGE('',*,*,#3812,.T.);
#4813=ORIENTED_EDGE('',*,*,#3813,.F.);
#4814=ORIENTED_EDGE('',*,*,#3812,.F.);
#4815=ORIENTED_EDGE('',*,*,#3811,.T.);
#4816=ORIENTED_EDGE('',*,*,#3814,.F.);
#4817=ORIENTED_EDGE('',*,*,#3815,.F.);
#4818=ORIENTED_EDGE('',*,*,#3816,.T.);
#4819=ORIENTED_EDGE('',*,*,#3817,.F.);
#4820=ORIENTED_EDGE('',*,*,#3816,.F.);
#4821=ORIENTED_EDGE('',*,*,#3815,.T.);
#4822=ORIENTED_EDGE('',*,*,#3818,.F.);
#4823=ORIENTED_EDGE('',*,*,#3819,.F.);
#4824=ORIENTED_EDGE('',*,*,#3820,.T.);
#4825=ORIENTED_EDGE('',*,*,#3821,.F.);
#4826=ORIENTED_EDGE('',*,*,#3820,.F.);
#4827=ORIENTED_EDGE('',*,*,#3819,.T.);
#4828=ORIENTED_EDGE('',*,*,#3822,.F.);
#4829=ORIENTED_EDGE('',*,*,#3823,.F.);
#4830=ORIENTED_EDGE('',*,*,#3824,.T.);
#4831=ORIENTED_EDGE('',*,*,#3810,.T.);
#4832=ORIENTED_EDGE('',*,*,#3824,.F.);
#4833=ORIENTED_EDGE('',*,*,#3825,.F.);
#4834=ORIENTED_EDGE('',*,*,#3826,.T.);
#4835=ORIENTED_EDGE('',*,*,#3814,.T.);
#4836=ORIENTED_EDGE('',*,*,#3826,.F.);
#4837=ORIENTED_EDGE('',*,*,#3827,.F.);
#4838=ORIENTED_EDGE('',*,*,#3828,.T.);
#4839=ORIENTED_EDGE('',*,*,#3818,.T.);
#4840=ORIENTED_EDGE('',*,*,#3828,.F.);
#4841=ORIENTED_EDGE('',*,*,#3829,.F.);
#4842=ORIENTED_EDGE('',*,*,#3830,.T.);
#4843=ORIENTED_EDGE('',*,*,#3822,.T.);
#4844=ORIENTED_EDGE('',*,*,#3830,.F.);
#4845=ORIENTED_EDGE('',*,*,#3831,.F.);
#4846=ORIENTED_EDGE('',*,*,#3832,.T.);
#4847=ORIENTED_EDGE('',*,*,#3833,.T.);
#4848=ORIENTED_EDGE('',*,*,#3832,.F.);
#4849=ORIENTED_EDGE('',*,*,#3833,.F.);
#4850=ORIENTED_EDGE('',*,*,#3834,.F.);
#4851=ORIENTED_EDGE('',*,*,#3835,.F.);
#4852=ORIENTED_EDGE('',*,*,#3836,.T.);
#4853=ORIENTED_EDGE('',*,*,#3834,.T.);
#4854=ORIENTED_EDGE('',*,*,#3836,.F.);
#4855=ORIENTED_EDGE('',*,*,#3837,.F.);
#4856=ORIENTED_EDGE('',*,*,#3838,.T.);
#4857=ORIENTED_EDGE('',*,*,#3839,.T.);
#4858=ORIENTED_EDGE('',*,*,#3838,.F.);
#4859=ORIENTED_EDGE('',*,*,#3837,.T.);
#4860=ORIENTED_EDGE('',*,*,#3835,.T.);
#4861=ORIENTED_EDGE('',*,*,#3821,.T.);
#4862=ORIENTED_EDGE('',*,*,#3817,.T.);
#4863=ORIENTED_EDGE('',*,*,#3813,.T.);
#4864=ORIENTED_EDGE('',*,*,#3809,.T.);
#4865=ORIENTED_EDGE('',*,*,#3839,.F.);
#4866=ORIENTED_EDGE('',*,*,#3831,.T.);
#4867=ORIENTED_EDGE('',*,*,#3829,.T.);
#4868=ORIENTED_EDGE('',*,*,#3827,.T.);
#4869=ORIENTED_EDGE('',*,*,#3825,.T.);
#4870=ORIENTED_EDGE('',*,*,#3823,.T.);
#4871=ORIENTED_EDGE('',*,*,#3840,.T.);
#4872=ORIENTED_EDGE('',*,*,#3841,.T.);
#4873=ORIENTED_EDGE('',*,*,#3842,.F.);
#4874=ORIENTED_EDGE('',*,*,#3843,.F.);
#4875=ORIENTED_EDGE('',*,*,#3844,.T.);
#4876=ORIENTED_EDGE('',*,*,#3843,.T.);
#4877=ORIENTED_EDGE('',*,*,#3845,.F.);
#4878=ORIENTED_EDGE('',*,*,#3846,.F.);
#4879=ORIENTED_EDGE('',*,*,#3847,.T.);
#4880=ORIENTED_EDGE('',*,*,#3846,.T.);
#4881=ORIENTED_EDGE('',*,*,#3848,.F.);
#4882=ORIENTED_EDGE('',*,*,#3849,.F.);
#4883=ORIENTED_EDGE('',*,*,#3850,.T.);
#4884=ORIENTED_EDGE('',*,*,#3849,.T.);
#4885=ORIENTED_EDGE('',*,*,#3851,.F.);
#4886=ORIENTED_EDGE('',*,*,#3841,.F.);
#4887=ORIENTED_EDGE('',*,*,#3851,.T.);
#4888=ORIENTED_EDGE('',*,*,#3848,.T.);
#4889=ORIENTED_EDGE('',*,*,#3845,.T.);
#4890=ORIENTED_EDGE('',*,*,#3842,.T.);
#4891=ORIENTED_EDGE('',*,*,#3850,.F.);
#4892=ORIENTED_EDGE('',*,*,#3840,.F.);
#4893=ORIENTED_EDGE('',*,*,#3844,.F.);
#4894=ORIENTED_EDGE('',*,*,#3847,.F.);
#4895=ORIENTED_EDGE('',*,*,#3852,.F.);
#4896=ORIENTED_EDGE('',*,*,#3853,.T.);
#4897=ORIENTED_EDGE('',*,*,#3854,.T.);
#4898=ORIENTED_EDGE('',*,*,#3853,.F.);
#4899=ORIENTED_EDGE('',*,*,#3854,.F.);
#4900=ORIENTED_EDGE('',*,*,#3855,.F.);
#4901=ORIENTED_EDGE('',*,*,#3856,.T.);
#4902=ORIENTED_EDGE('',*,*,#3857,.T.);
#4903=ORIENTED_EDGE('',*,*,#3856,.F.);
#4904=ORIENTED_EDGE('',*,*,#3857,.F.);
#4905=ORIENTED_EDGE('',*,*,#3858,.T.);
#4906=ORIENTED_EDGE('',*,*,#3859,.T.);
#4907=ORIENTED_EDGE('',*,*,#3860,.F.);
#4908=ORIENTED_EDGE('',*,*,#3861,.F.);
#4909=ORIENTED_EDGE('',*,*,#3862,.T.);
#4910=ORIENTED_EDGE('',*,*,#3861,.T.);
#4911=ORIENTED_EDGE('',*,*,#3863,.F.);
#4912=ORIENTED_EDGE('',*,*,#3864,.F.);
#4913=ORIENTED_EDGE('',*,*,#3865,.T.);
#4914=ORIENTED_EDGE('',*,*,#3864,.T.);
#4915=ORIENTED_EDGE('',*,*,#3866,.F.);
#4916=ORIENTED_EDGE('',*,*,#3867,.F.);
#4917=ORIENTED_EDGE('',*,*,#3868,.T.);
#4918=ORIENTED_EDGE('',*,*,#3867,.T.);
#4919=ORIENTED_EDGE('',*,*,#3869,.F.);
#4920=ORIENTED_EDGE('',*,*,#3859,.F.);
#4921=ORIENTED_EDGE('',*,*,#3869,.T.);
#4922=ORIENTED_EDGE('',*,*,#3866,.T.);
#4923=ORIENTED_EDGE('',*,*,#3863,.T.);
#4924=ORIENTED_EDGE('',*,*,#3860,.T.);
#4925=ORIENTED_EDGE('',*,*,#3868,.F.);
#4926=ORIENTED_EDGE('',*,*,#3858,.F.);
#4927=ORIENTED_EDGE('',*,*,#3862,.F.);
#4928=ORIENTED_EDGE('',*,*,#3865,.F.);
#4929=ORIENTED_EDGE('',*,*,#3852,.T.);
#4930=ORIENTED_EDGE('',*,*,#3855,.T.);
#4931=ORIENTED_EDGE('',*,*,#3870,.F.);
#4932=ORIENTED_EDGE('',*,*,#3871,.T.);
#4933=ORIENTED_EDGE('',*,*,#3872,.T.);
#4934=ORIENTED_EDGE('',*,*,#3871,.F.);
#4935=ORIENTED_EDGE('',*,*,#3872,.F.);
#4936=ORIENTED_EDGE('',*,*,#3873,.F.);
#4937=ORIENTED_EDGE('',*,*,#3874,.T.);
#4938=ORIENTED_EDGE('',*,*,#3875,.T.);
#4939=ORIENTED_EDGE('',*,*,#3874,.F.);
#4940=ORIENTED_EDGE('',*,*,#3875,.F.);
#4941=ORIENTED_EDGE('',*,*,#3876,.T.);
#4942=ORIENTED_EDGE('',*,*,#3877,.T.);
#4943=ORIENTED_EDGE('',*,*,#3878,.F.);
#4944=ORIENTED_EDGE('',*,*,#3879,.F.);
#4945=ORIENTED_EDGE('',*,*,#3880,.T.);
#4946=ORIENTED_EDGE('',*,*,#3879,.T.);
#4947=ORIENTED_EDGE('',*,*,#3881,.F.);
#4948=ORIENTED_EDGE('',*,*,#3882,.F.);
#4949=ORIENTED_EDGE('',*,*,#3883,.T.);
#4950=ORIENTED_EDGE('',*,*,#3882,.T.);
#4951=ORIENTED_EDGE('',*,*,#3884,.F.);
#4952=ORIENTED_EDGE('',*,*,#3885,.F.);
#4953=ORIENTED_EDGE('',*,*,#3886,.T.);
#4954=ORIENTED_EDGE('',*,*,#3885,.T.);
#4955=ORIENTED_EDGE('',*,*,#3887,.F.);
#4956=ORIENTED_EDGE('',*,*,#3877,.F.);
#4957=ORIENTED_EDGE('',*,*,#3887,.T.);
#4958=ORIENTED_EDGE('',*,*,#3884,.T.);
#4959=ORIENTED_EDGE('',*,*,#3881,.T.);
#4960=ORIENTED_EDGE('',*,*,#3878,.T.);
#4961=ORIENTED_EDGE('',*,*,#3886,.F.);
#4962=ORIENTED_EDGE('',*,*,#3876,.F.);
#4963=ORIENTED_EDGE('',*,*,#3880,.F.);
#4964=ORIENTED_EDGE('',*,*,#3883,.F.);
#4965=ORIENTED_EDGE('',*,*,#3870,.T.);
#4966=ORIENTED_EDGE('',*,*,#3873,.T.);
#4967=ORIENTED_EDGE('',*,*,#3888,.F.);
#4968=ORIENTED_EDGE('',*,*,#3889,.T.);
#4969=ORIENTED_EDGE('',*,*,#3890,.F.);
#4970=ORIENTED_EDGE('',*,*,#3889,.F.);
#4971=ORIENTED_EDGE('',*,*,#3888,.T.);
#4972=ORIENTED_EDGE('',*,*,#3891,.F.);
#4973=ORIENTED_EDGE('',*,*,#3892,.T.);
#4974=ORIENTED_EDGE('',*,*,#3893,.F.);
#4975=ORIENTED_EDGE('',*,*,#3894,.T.);
#4976=ORIENTED_EDGE('',*,*,#3891,.T.);
#4977=ORIENTED_EDGE('',*,*,#3894,.F.);
#4978=ORIENTED_EDGE('',*,*,#3893,.T.);
#4979=ORIENTED_EDGE('',*,*,#3890,.T.);
#4980=ORIENTED_EDGE('',*,*,#3892,.F.);
#4981=ORIENTED_EDGE('',*,*,#3895,.T.);
#4982=ORIENTED_EDGE('',*,*,#3896,.T.);
#4983=ORIENTED_EDGE('',*,*,#3895,.F.);
#4984=ORIENTED_EDGE('',*,*,#3896,.F.);
#4985=ORIENTED_EDGE('',*,*,#3897,.T.);
#4986=ORIENTED_EDGE('',*,*,#3898,.T.);
#4987=ORIENTED_EDGE('',*,*,#3899,.T.);
#4988=ORIENTED_EDGE('',*,*,#3900,.F.);
#4989=ORIENTED_EDGE('',*,*,#3901,.T.);
#4990=ORIENTED_EDGE('',*,*,#3902,.T.);
#4991=ORIENTED_EDGE('',*,*,#3903,.T.);
#4992=ORIENTED_EDGE('',*,*,#3898,.F.);
#4993=ORIENTED_EDGE('',*,*,#3904,.T.);
#4994=ORIENTED_EDGE('',*,*,#3905,.T.);
#4995=ORIENTED_EDGE('',*,*,#3906,.T.);
#4996=ORIENTED_EDGE('',*,*,#3902,.F.);
#4997=ORIENTED_EDGE('',*,*,#3907,.T.);
#4998=ORIENTED_EDGE('',*,*,#3908,.T.);
#4999=ORIENTED_EDGE('',*,*,#3909,.T.);
#5000=ORIENTED_EDGE('',*,*,#3905,.F.);
#5001=ORIENTED_EDGE('',*,*,#3910,.T.);
#5002=ORIENTED_EDGE('',*,*,#3911,.T.);
#5003=ORIENTED_EDGE('',*,*,#3912,.T.);
#5004=ORIENTED_EDGE('',*,*,#3908,.F.);
#5005=ORIENTED_EDGE('',*,*,#3913,.T.);
#5006=ORIENTED_EDGE('',*,*,#3900,.T.);
#5007=ORIENTED_EDGE('',*,*,#3914,.T.);
#5008=ORIENTED_EDGE('',*,*,#3911,.F.);
#5009=ORIENTED_EDGE('',*,*,#3913,.F.);
#5010=ORIENTED_EDGE('',*,*,#3910,.F.);
#5011=ORIENTED_EDGE('',*,*,#3907,.F.);
#5012=ORIENTED_EDGE('',*,*,#3904,.F.);
#5013=ORIENTED_EDGE('',*,*,#3901,.F.);
#5014=ORIENTED_EDGE('',*,*,#3897,.F.);
#5015=ORIENTED_EDGE('',*,*,#3914,.F.);
#5016=ORIENTED_EDGE('',*,*,#3899,.F.);
#5017=ORIENTED_EDGE('',*,*,#3903,.F.);
#5018=ORIENTED_EDGE('',*,*,#3906,.F.);
#5019=ORIENTED_EDGE('',*,*,#3909,.F.);
#5020=ORIENTED_EDGE('',*,*,#3912,.F.);
#5021=ORIENTED_EDGE('',*,*,#3915,.F.);
#5022=ORIENTED_EDGE('',*,*,#3916,.F.);
#5023=ORIENTED_EDGE('',*,*,#3917,.F.);
#5024=ORIENTED_EDGE('',*,*,#3918,.T.);
#5025=ORIENTED_EDGE('',*,*,#3916,.T.);
#5026=ORIENTED_EDGE('',*,*,#3918,.F.);
#5027=ORIENTED_EDGE('',*,*,#3919,.F.);
#5028=ORIENTED_EDGE('',*,*,#3920,.T.);
#5029=ORIENTED_EDGE('',*,*,#3917,.T.);
#5030=ORIENTED_EDGE('',*,*,#3920,.F.);
#5031=ORIENTED_EDGE('',*,*,#3921,.F.);
#5032=ORIENTED_EDGE('',*,*,#3922,.T.);
#5033=ORIENTED_EDGE('',*,*,#3919,.T.);
#5034=ORIENTED_EDGE('',*,*,#3922,.F.);
#5035=ORIENTED_EDGE('',*,*,#3921,.T.);
#5036=ORIENTED_EDGE('',*,*,#3923,.F.);
#5037=ORIENTED_EDGE('',*,*,#3924,.F.);
#5038=ORIENTED_EDGE('',*,*,#3925,.T.);
#5039=ORIENTED_EDGE('',*,*,#3923,.T.);
#5040=ORIENTED_EDGE('',*,*,#3925,.F.);
#5041=ORIENTED_EDGE('',*,*,#3915,.T.);
#5042=ORIENTED_EDGE('',*,*,#3926,.T.);
#5043=ORIENTED_EDGE('',*,*,#3924,.T.);
#5044=ORIENTED_EDGE('',*,*,#3926,.F.);
#5045=ORIENTED_EDGE('',*,*,#3927,.F.);
#5046=ORIENTED_EDGE('',*,*,#3928,.F.);
#5047=ORIENTED_EDGE('',*,*,#3929,.T.);
#5048=ORIENTED_EDGE('',*,*,#3930,.F.);
#5049=ORIENTED_EDGE('',*,*,#3931,.F.);
#5050=ORIENTED_EDGE('',*,*,#3929,.F.);
#5051=ORIENTED_EDGE('',*,*,#3930,.T.);
#5052=ORIENTED_EDGE('',*,*,#3931,.T.);
#5053=ORIENTED_EDGE('',*,*,#3932,.T.);
#5054=ORIENTED_EDGE('',*,*,#3933,.T.);
#5055=ORIENTED_EDGE('',*,*,#3932,.F.);
#5056=ORIENTED_EDGE('',*,*,#3934,.T.);
#5057=ORIENTED_EDGE('',*,*,#3935,.T.);
#5058=ORIENTED_EDGE('',*,*,#3936,.F.);
#5059=ORIENTED_EDGE('',*,*,#3935,.F.);
#5060=ORIENTED_EDGE('',*,*,#3936,.T.);
#5061=ORIENTED_EDGE('',*,*,#3937,.T.);
#5062=ORIENTED_EDGE('',*,*,#3938,.F.);
#5063=ORIENTED_EDGE('',*,*,#3937,.F.);
#5064=ORIENTED_EDGE('',*,*,#3933,.F.);
#5065=ORIENTED_EDGE('',*,*,#3938,.T.);
#5066=ORIENTED_EDGE('',*,*,#3939,.F.);
#5067=ORIENTED_EDGE('',*,*,#3940,.T.);
#5068=ORIENTED_EDGE('',*,*,#3927,.T.);
#5069=ORIENTED_EDGE('',*,*,#3928,.T.);
#5070=ORIENTED_EDGE('',*,*,#3940,.F.);
#5071=ORIENTED_EDGE('',*,*,#3939,.T.);
#5072=ORIENTED_EDGE('',*,*,#3941,.F.);
#5073=ORIENTED_EDGE('',*,*,#3941,.T.);
#5074=ORIENTED_EDGE('',*,*,#3942,.T.);
#5075=ORIENTED_EDGE('',*,*,#3934,.F.);
#5076=ORIENTED_EDGE('',*,*,#3942,.F.);
#5077=ORIENTED_EDGE('',*,*,#3943,.F.);
#5078=ORIENTED_EDGE('',*,*,#3944,.F.);
#5079=ORIENTED_EDGE('',*,*,#3945,.T.);
#5080=ORIENTED_EDGE('',*,*,#3946,.F.);
#5081=ORIENTED_EDGE('',*,*,#3947,.F.);
#5082=ORIENTED_EDGE('',*,*,#3945,.F.);
#5083=ORIENTED_EDGE('',*,*,#3948,.T.);
#5084=ORIENTED_EDGE('',*,*,#3949,.T.);
#5085=ORIENTED_EDGE('',*,*,#3946,.T.);
#5086=ORIENTED_EDGE('',*,*,#3947,.T.);
#5087=ORIENTED_EDGE('',*,*,#3949,.F.);
#5088=ORIENTED_EDGE('',*,*,#3950,.F.);
#5089=ORIENTED_EDGE('',*,*,#3951,.T.);
#5090=ORIENTED_EDGE('',*,*,#3952,.F.);
#5091=ORIENTED_EDGE('',*,*,#3953,.T.);
#5092=ORIENTED_EDGE('',*,*,#3950,.T.);
#5093=ORIENTED_EDGE('',*,*,#3953,.F.);
#5094=ORIENTED_EDGE('',*,*,#3954,.F.);
#5095=ORIENTED_EDGE('',*,*,#3955,.T.);
#5096=ORIENTED_EDGE('',*,*,#3952,.T.);
#5097=ORIENTED_EDGE('',*,*,#3955,.F.);
#5098=ORIENTED_EDGE('',*,*,#3956,.F.);
#5099=ORIENTED_EDGE('',*,*,#3957,.T.);
#5100=ORIENTED_EDGE('',*,*,#3954,.T.);
#5101=ORIENTED_EDGE('',*,*,#3957,.F.);
#5102=ORIENTED_EDGE('',*,*,#3956,.T.);
#5103=ORIENTED_EDGE('',*,*,#3948,.F.);
#5104=ORIENTED_EDGE('',*,*,#3943,.T.);
#5105=ORIENTED_EDGE('',*,*,#3944,.T.);
#5106=ORIENTED_EDGE('',*,*,#3958,.T.);
#5107=ORIENTED_EDGE('',*,*,#3951,.F.);
#5108=ORIENTED_EDGE('',*,*,#3958,.F.);
#5109=ORIENTED_EDGE('',*,*,#3959,.T.);
#5110=ORIENTED_EDGE('',*,*,#3959,.F.);
#5111=ORIENTED_EDGE('',*,*,#3960,.T.);
#5112=ORIENTED_EDGE('',*,*,#3960,.F.);
#5113=ORIENTED_EDGE('',*,*,#3961,.T.);
#5114=ORIENTED_EDGE('',*,*,#3961,.F.);
#5115=ORIENTED_EDGE('',*,*,#3962,.T.);
#5116=ORIENTED_EDGE('',*,*,#3962,.F.);
#5117=ORIENTED_EDGE('',*,*,#3963,.T.);
#5118=ORIENTED_EDGE('',*,*,#3963,.F.);
#5119=ORIENTED_EDGE('',*,*,#3964,.T.);
#5120=ORIENTED_EDGE('',*,*,#3964,.F.);
#5121=ORIENTED_EDGE('',*,*,#3965,.T.);
#5122=ORIENTED_EDGE('',*,*,#3965,.F.);
#5123=ORIENTED_EDGE('',*,*,#3966,.T.);
#5124=ORIENTED_EDGE('',*,*,#3966,.F.);
#5125=ORIENTED_EDGE('',*,*,#3967,.F.);
#5126=ORIENTED_EDGE('',*,*,#3968,.F.);
#5127=ORIENTED_EDGE('',*,*,#3969,.F.);
#5128=ORIENTED_EDGE('',*,*,#3970,.F.);
#5129=ORIENTED_EDGE('',*,*,#3969,.T.);
#5130=ORIENTED_EDGE('',*,*,#3971,.F.);
#5131=ORIENTED_EDGE('',*,*,#3972,.T.);
#5132=ORIENTED_EDGE('',*,*,#3973,.F.);
#5133=ORIENTED_EDGE('',*,*,#3974,.T.);
#5134=ORIENTED_EDGE('',*,*,#3975,.F.);
#5135=ORIENTED_EDGE('',*,*,#3976,.T.);
#5136=ORIENTED_EDGE('',*,*,#3977,.T.);
#5137=ORIENTED_EDGE('',*,*,#3978,.F.);
#5138=ORIENTED_EDGE('',*,*,#3977,.F.);
#5139=ORIENTED_EDGE('',*,*,#3979,.T.);
#5140=ORIENTED_EDGE('',*,*,#3980,.F.);
#5141=ORIENTED_EDGE('',*,*,#3981,.T.);
#5142=ORIENTED_EDGE('',*,*,#3982,.F.);
#5143=ORIENTED_EDGE('',*,*,#3983,.T.);
#5144=ORIENTED_EDGE('',*,*,#3984,.F.);
#5145=ORIENTED_EDGE('',*,*,#3985,.T.);
#5146=ORIENTED_EDGE('',*,*,#3986,.F.);
#5147=ORIENTED_EDGE('',*,*,#3987,.T.);
#5148=ORIENTED_EDGE('',*,*,#3988,.F.);
#5149=ORIENTED_EDGE('',*,*,#3968,.T.);
#5150=ORIENTED_EDGE('',*,*,#3989,.T.);
#5151=ORIENTED_EDGE('',*,*,#3990,.T.);
#5152=ORIENTED_EDGE('',*,*,#3971,.T.);
#5153=ORIENTED_EDGE('',*,*,#3991,.F.);
#5154=ORIENTED_EDGE('',*,*,#3992,.F.);
#5155=ORIENTED_EDGE('',*,*,#3972,.F.);
#5156=ORIENTED_EDGE('',*,*,#3990,.F.);
#5157=ORIENTED_EDGE('',*,*,#3992,.T.);
#5158=ORIENTED_EDGE('',*,*,#3993,.T.);
#5159=ORIENTED_EDGE('',*,*,#3994,.T.);
#5160=ORIENTED_EDGE('',*,*,#3973,.T.);
#5161=ORIENTED_EDGE('',*,*,#3995,.F.);
#5162=ORIENTED_EDGE('',*,*,#3996,.F.);
#5163=ORIENTED_EDGE('',*,*,#3974,.F.);
#5164=ORIENTED_EDGE('',*,*,#3994,.F.);
#5165=ORIENTED_EDGE('',*,*,#3996,.T.);
#5166=ORIENTED_EDGE('',*,*,#3997,.T.);
#5167=ORIENTED_EDGE('',*,*,#3998,.T.);
#5168=ORIENTED_EDGE('',*,*,#3975,.T.);
#5169=ORIENTED_EDGE('',*,*,#3999,.F.);
#5170=ORIENTED_EDGE('',*,*,#4000,.F.);
#5171=ORIENTED_EDGE('',*,*,#3979,.F.);
#5172=ORIENTED_EDGE('',*,*,#3976,.F.);
#5173=ORIENTED_EDGE('',*,*,#3998,.F.);
#5174=ORIENTED_EDGE('',*,*,#4001,.F.);
#5175=ORIENTED_EDGE('',*,*,#4000,.T.);
#5176=ORIENTED_EDGE('',*,*,#4002,.T.);
#5177=ORIENTED_EDGE('',*,*,#4003,.T.);
#5178=ORIENTED_EDGE('',*,*,#3980,.T.);
#5179=ORIENTED_EDGE('',*,*,#4004,.F.);
#5180=ORIENTED_EDGE('',*,*,#4005,.F.);
#5181=ORIENTED_EDGE('',*,*,#3981,.F.);
#5182=ORIENTED_EDGE('',*,*,#4003,.F.);
#5183=ORIENTED_EDGE('',*,*,#4005,.T.);
#5184=ORIENTED_EDGE('',*,*,#4006,.T.);
#5185=ORIENTED_EDGE('',*,*,#4007,.T.);
#5186=ORIENTED_EDGE('',*,*,#3982,.T.);
#5187=ORIENTED_EDGE('',*,*,#4008,.F.);
#5188=ORIENTED_EDGE('',*,*,#4009,.F.);
#5189=ORIENTED_EDGE('',*,*,#3983,.F.);
#5190=ORIENTED_EDGE('',*,*,#4007,.F.);
#5191=ORIENTED_EDGE('',*,*,#4009,.T.);
#5192=ORIENTED_EDGE('',*,*,#4010,.T.);
#5193=ORIENTED_EDGE('',*,*,#4011,.T.);
#5194=ORIENTED_EDGE('',*,*,#3984,.T.);
#5195=ORIENTED_EDGE('',*,*,#3985,.F.);
#5196=ORIENTED_EDGE('',*,*,#4011,.F.);
#5197=ORIENTED_EDGE('',*,*,#4012,.F.);
#5198=ORIENTED_EDGE('',*,*,#4013,.F.);
#5199=ORIENTED_EDGE('',*,*,#4014,.F.);
#5200=ORIENTED_EDGE('',*,*,#4015,.T.);
#5201=ORIENTED_EDGE('',*,*,#4001,.T.);
#5202=ORIENTED_EDGE('',*,*,#3997,.F.);
#5203=ORIENTED_EDGE('',*,*,#3995,.T.);
#5204=ORIENTED_EDGE('',*,*,#3993,.F.);
#5205=ORIENTED_EDGE('',*,*,#3991,.T.);
#5206=ORIENTED_EDGE('',*,*,#3989,.F.);
#5207=ORIENTED_EDGE('',*,*,#3967,.T.);
#5208=ORIENTED_EDGE('',*,*,#4016,.F.);
#5209=ORIENTED_EDGE('',*,*,#4017,.T.);
#5210=ORIENTED_EDGE('',*,*,#4018,.F.);
#5211=ORIENTED_EDGE('',*,*,#4012,.T.);
#5212=ORIENTED_EDGE('',*,*,#4010,.F.);
#5213=ORIENTED_EDGE('',*,*,#4008,.T.);
#5214=ORIENTED_EDGE('',*,*,#4006,.F.);
#5215=ORIENTED_EDGE('',*,*,#4004,.T.);
#5216=ORIENTED_EDGE('',*,*,#4002,.F.);
#5217=ORIENTED_EDGE('',*,*,#3999,.T.);
#5218=ORIENTED_EDGE('',*,*,#4015,.F.);
#5219=ORIENTED_EDGE('',*,*,#3970,.T.);
#5220=ORIENTED_EDGE('',*,*,#3988,.T.);
#5221=ORIENTED_EDGE('',*,*,#4019,.T.);
#5222=ORIENTED_EDGE('',*,*,#4016,.T.);
#5223=ORIENTED_EDGE('',*,*,#3987,.F.);
#5224=ORIENTED_EDGE('',*,*,#4020,.F.);
#5225=ORIENTED_EDGE('',*,*,#4017,.F.);
#5226=ORIENTED_EDGE('',*,*,#4019,.F.);
#5227=ORIENTED_EDGE('',*,*,#3978,.T.);
#5228=ORIENTED_EDGE('',*,*,#4014,.T.);
#5229=ORIENTED_EDGE('',*,*,#4013,.T.);
#5230=ORIENTED_EDGE('',*,*,#4018,.T.);
#5231=ORIENTED_EDGE('',*,*,#4020,.T.);
#5232=ORIENTED_EDGE('',*,*,#3986,.T.);
#5233=ORIENTED_EDGE('',*,*,#4021,.F.);
#5234=ORIENTED_EDGE('',*,*,#4022,.T.);
#5235=ORIENTED_EDGE('',*,*,#4023,.F.);
#5236=ORIENTED_EDGE('',*,*,#4024,.T.);
#5237=ORIENTED_EDGE('',*,*,#4021,.T.);
#5238=ORIENTED_EDGE('',*,*,#4024,.F.);
#5239=ORIENTED_EDGE('',*,*,#4023,.T.);
#5240=ORIENTED_EDGE('',*,*,#4025,.F.);
#5241=ORIENTED_EDGE('',*,*,#4025,.T.);
#5242=ORIENTED_EDGE('',*,*,#4026,.T.);
#5243=ORIENTED_EDGE('',*,*,#4022,.F.);
#5244=ORIENTED_EDGE('',*,*,#4026,.F.);
#5245=ORIENTED_EDGE('',*,*,#4027,.F.);
#5246=ORIENTED_EDGE('',*,*,#4028,.T.);
#5247=ORIENTED_EDGE('',*,*,#4029,.F.);
#5248=ORIENTED_EDGE('',*,*,#4030,.T.);
#5249=ORIENTED_EDGE('',*,*,#4027,.T.);
#5250=ORIENTED_EDGE('',*,*,#4030,.F.);
#5251=ORIENTED_EDGE('',*,*,#4029,.T.);
#5252=ORIENTED_EDGE('',*,*,#4031,.F.);
#5253=ORIENTED_EDGE('',*,*,#4031,.T.);
#5254=ORIENTED_EDGE('',*,*,#4032,.T.);
#5255=ORIENTED_EDGE('',*,*,#4028,.F.);
#5256=ORIENTED_EDGE('',*,*,#4032,.F.);
#5257=ORIENTED_EDGE('',*,*,#4033,.F.);
#5258=ORIENTED_EDGE('',*,*,#4034,.F.);
#5259=ORIENTED_EDGE('',*,*,#4035,.F.);
#5260=ORIENTED_EDGE('',*,*,#4036,.F.);
#5261=ORIENTED_EDGE('',*,*,#4037,.F.);
#5262=ORIENTED_EDGE('',*,*,#4036,.T.);
#5263=ORIENTED_EDGE('',*,*,#4038,.F.);
#5264=ORIENTED_EDGE('',*,*,#4039,.T.);
#5265=ORIENTED_EDGE('',*,*,#4040,.F.);
#5266=ORIENTED_EDGE('',*,*,#4039,.F.);
#5267=ORIENTED_EDGE('',*,*,#4041,.F.);
#5268=ORIENTED_EDGE('',*,*,#4042,.F.);
#5269=ORIENTED_EDGE('',*,*,#4043,.F.);
#5270=ORIENTED_EDGE('',*,*,#4042,.T.);
#5271=ORIENTED_EDGE('',*,*,#4044,.T.);
#5272=ORIENTED_EDGE('',*,*,#4034,.T.);
#5273=ORIENTED_EDGE('',*,*,#4044,.F.);
#5274=ORIENTED_EDGE('',*,*,#4041,.T.);
#5275=ORIENTED_EDGE('',*,*,#4038,.T.);
#5276=ORIENTED_EDGE('',*,*,#4035,.T.);
#5277=ORIENTED_EDGE('',*,*,#4045,.F.);
#5278=ORIENTED_EDGE('',*,*,#4046,.T.);
#5279=ORIENTED_EDGE('',*,*,#4047,.F.);
#5280=ORIENTED_EDGE('',*,*,#4048,.T.);
#5281=ORIENTED_EDGE('',*,*,#4045,.T.);
#5282=ORIENTED_EDGE('',*,*,#4048,.F.);
#5283=ORIENTED_EDGE('',*,*,#4047,.T.);
#5284=ORIENTED_EDGE('',*,*,#4049,.F.);
#5285=ORIENTED_EDGE('',*,*,#4050,.F.);
#5286=ORIENTED_EDGE('',*,*,#4051,.T.);
#5287=ORIENTED_EDGE('',*,*,#4049,.T.);
#5288=ORIENTED_EDGE('',*,*,#4051,.F.);
#5289=ORIENTED_EDGE('',*,*,#4052,.F.);
#5290=ORIENTED_EDGE('',*,*,#4050,.T.);
#5291=ORIENTED_EDGE('',*,*,#4053,.F.);
#5292=ORIENTED_EDGE('',*,*,#4054,.T.);
#5293=ORIENTED_EDGE('',*,*,#4052,.T.);
#5294=ORIENTED_EDGE('',*,*,#4054,.F.);
#5295=ORIENTED_EDGE('',*,*,#4053,.T.);
#5296=ORIENTED_EDGE('',*,*,#4055,.F.);
#5297=ORIENTED_EDGE('',*,*,#4056,.F.);
#5298=ORIENTED_EDGE('',*,*,#4057,.T.);
#5299=ORIENTED_EDGE('',*,*,#4055,.T.);
#5300=ORIENTED_EDGE('',*,*,#4057,.F.);
#5301=ORIENTED_EDGE('',*,*,#4058,.F.);
#5302=ORIENTED_EDGE('',*,*,#4056,.T.);
#5303=ORIENTED_EDGE('',*,*,#4059,.F.);
#5304=ORIENTED_EDGE('',*,*,#4060,.T.);
#5305=ORIENTED_EDGE('',*,*,#4058,.T.);
#5306=ORIENTED_EDGE('',*,*,#4060,.F.);
#5307=ORIENTED_EDGE('',*,*,#4059,.T.);
#5308=ORIENTED_EDGE('',*,*,#4061,.F.);
#5309=ORIENTED_EDGE('',*,*,#4061,.T.);
#5310=ORIENTED_EDGE('',*,*,#4062,.T.);
#5311=ORIENTED_EDGE('',*,*,#4046,.F.);
#5312=ORIENTED_EDGE('',*,*,#4062,.F.);
#5313=ORIENTED_EDGE('',*,*,#4040,.T.);
#5314=ORIENTED_EDGE('',*,*,#4043,.T.);
#5315=ORIENTED_EDGE('',*,*,#4033,.T.);
#5316=ORIENTED_EDGE('',*,*,#4037,.T.);
#5317=ORIENTED_EDGE('',*,*,#4063,.F.);
#5318=ORIENTED_EDGE('',*,*,#4064,.F.);
#5319=ORIENTED_EDGE('',*,*,#4065,.F.);
#5320=ORIENTED_EDGE('',*,*,#4066,.F.);
#5321=ORIENTED_EDGE('',*,*,#4067,.F.);
#5322=ORIENTED_EDGE('',*,*,#4066,.T.);
#5323=ORIENTED_EDGE('',*,*,#4068,.F.);
#5324=ORIENTED_EDGE('',*,*,#4069,.T.);
#5325=ORIENTED_EDGE('',*,*,#4070,.F.);
#5326=ORIENTED_EDGE('',*,*,#4069,.F.);
#5327=ORIENTED_EDGE('',*,*,#4071,.F.);
#5328=ORIENTED_EDGE('',*,*,#4072,.F.);
#5329=ORIENTED_EDGE('',*,*,#4073,.F.);
#5330=ORIENTED_EDGE('',*,*,#4072,.T.);
#5331=ORIENTED_EDGE('',*,*,#4074,.F.);
#5332=ORIENTED_EDGE('',*,*,#4064,.T.);
#5333=ORIENTED_EDGE('',*,*,#4075,.F.);
#5334=ORIENTED_EDGE('',*,*,#4076,.T.);
#5335=ORIENTED_EDGE('',*,*,#4077,.F.);
#5336=ORIENTED_EDGE('',*,*,#4078,.T.);
#5337=ORIENTED_EDGE('',*,*,#4075,.T.);
#5338=ORIENTED_EDGE('',*,*,#4078,.F.);
#5339=ORIENTED_EDGE('',*,*,#4070,.T.);
#5340=ORIENTED_EDGE('',*,*,#4073,.T.);
#5341=ORIENTED_EDGE('',*,*,#4063,.T.);
#5342=ORIENTED_EDGE('',*,*,#4067,.T.);
#5343=ORIENTED_EDGE('',*,*,#4077,.T.);
#5344=ORIENTED_EDGE('',*,*,#4079,.F.);
#5345=ORIENTED_EDGE('',*,*,#4079,.T.);
#5346=ORIENTED_EDGE('',*,*,#4080,.T.);
#5347=ORIENTED_EDGE('',*,*,#4076,.F.);
#5348=ORIENTED_EDGE('',*,*,#4080,.F.);
#5349=ORIENTED_EDGE('',*,*,#4071,.T.);
#5350=ORIENTED_EDGE('',*,*,#4068,.T.);
#5351=ORIENTED_EDGE('',*,*,#4065,.T.);
#5352=ORIENTED_EDGE('',*,*,#4074,.T.);
#5353=ORIENTED_EDGE('',*,*,#4081,.T.);
#5354=ORIENTED_EDGE('',*,*,#4082,.T.);
#5355=ORIENTED_EDGE('',*,*,#4083,.T.);
#5356=ORIENTED_EDGE('',*,*,#4084,.F.);
#5357=ORIENTED_EDGE('',*,*,#4085,.T.);
#5358=ORIENTED_EDGE('',*,*,#4086,.T.);
#5359=ORIENTED_EDGE('',*,*,#4087,.T.);
#5360=ORIENTED_EDGE('',*,*,#4082,.F.);
#5361=ORIENTED_EDGE('',*,*,#4088,.T.);
#5362=ORIENTED_EDGE('',*,*,#4089,.T.);
#5363=ORIENTED_EDGE('',*,*,#4090,.T.);
#5364=ORIENTED_EDGE('',*,*,#4086,.F.);
#5365=ORIENTED_EDGE('',*,*,#4091,.T.);
#5366=ORIENTED_EDGE('',*,*,#4092,.T.);
#5367=ORIENTED_EDGE('',*,*,#4093,.T.);
#5368=ORIENTED_EDGE('',*,*,#4089,.F.);
#5369=ORIENTED_EDGE('',*,*,#4094,.T.);
#5370=ORIENTED_EDGE('',*,*,#4095,.T.);
#5371=ORIENTED_EDGE('',*,*,#4096,.T.);
#5372=ORIENTED_EDGE('',*,*,#4092,.F.);
#5373=ORIENTED_EDGE('',*,*,#4097,.T.);
#5374=ORIENTED_EDGE('',*,*,#4084,.T.);
#5375=ORIENTED_EDGE('',*,*,#4098,.T.);
#5376=ORIENTED_EDGE('',*,*,#4095,.F.);
#5377=ORIENTED_EDGE('',*,*,#4097,.F.);
#5378=ORIENTED_EDGE('',*,*,#4094,.F.);
#5379=ORIENTED_EDGE('',*,*,#4091,.F.);
#5380=ORIENTED_EDGE('',*,*,#4088,.F.);
#5381=ORIENTED_EDGE('',*,*,#4085,.F.);
#5382=ORIENTED_EDGE('',*,*,#4081,.F.);
#5383=ORIENTED_EDGE('',*,*,#4098,.F.);
#5384=ORIENTED_EDGE('',*,*,#4083,.F.);
#5385=ORIENTED_EDGE('',*,*,#4087,.F.);
#5386=ORIENTED_EDGE('',*,*,#4090,.F.);
#5387=ORIENTED_EDGE('',*,*,#4093,.F.);
#5388=ORIENTED_EDGE('',*,*,#4096,.F.);
#5389=ORIENTED_EDGE('',*,*,#4099,.T.);
#5390=ORIENTED_EDGE('',*,*,#4100,.T.);
#5391=ORIENTED_EDGE('',*,*,#4099,.F.);
#5392=ORIENTED_EDGE('',*,*,#4101,.T.);
#5393=ORIENTED_EDGE('',*,*,#4102,.T.);
#5394=ORIENTED_EDGE('',*,*,#4101,.F.);
#5395=ORIENTED_EDGE('',*,*,#4102,.F.);
#5396=ORIENTED_EDGE('',*,*,#4103,.F.);
#5397=ORIENTED_EDGE('',*,*,#4104,.F.);
#5398=ORIENTED_EDGE('',*,*,#4105,.T.);
#5399=ORIENTED_EDGE('',*,*,#4103,.T.);
#5400=ORIENTED_EDGE('',*,*,#4105,.F.);
#5401=ORIENTED_EDGE('',*,*,#4106,.F.);
#5402=ORIENTED_EDGE('',*,*,#4107,.T.);
#5403=ORIENTED_EDGE('',*,*,#4104,.T.);
#5404=ORIENTED_EDGE('',*,*,#4107,.F.);
#5405=ORIENTED_EDGE('',*,*,#4108,.F.);
#5406=ORIENTED_EDGE('',*,*,#4109,.T.);
#5407=ORIENTED_EDGE('',*,*,#4106,.T.);
#5408=ORIENTED_EDGE('',*,*,#4109,.F.);
#5409=ORIENTED_EDGE('',*,*,#4108,.T.);
#5410=ORIENTED_EDGE('',*,*,#4110,.F.);
#5411=ORIENTED_EDGE('',*,*,#4111,.F.);
#5412=ORIENTED_EDGE('',*,*,#4112,.T.);
#5413=ORIENTED_EDGE('',*,*,#4110,.T.);
#5414=ORIENTED_EDGE('',*,*,#4112,.F.);
#5415=ORIENTED_EDGE('',*,*,#4113,.F.);
#5416=ORIENTED_EDGE('',*,*,#4114,.T.);
#5417=ORIENTED_EDGE('',*,*,#4111,.T.);
#5418=ORIENTED_EDGE('',*,*,#4114,.F.);
#5419=ORIENTED_EDGE('',*,*,#4100,.F.);
#5420=ORIENTED_EDGE('',*,*,#4115,.T.);
#5421=ORIENTED_EDGE('',*,*,#4113,.T.);
#5422=ORIENTED_EDGE('',*,*,#4115,.F.);
#5423=ORIENTED_EDGE('',*,*,#4116,.F.);
#5424=ORIENTED_EDGE('',*,*,#4117,.T.);
#5425=ORIENTED_EDGE('',*,*,#4118,.F.);
#5426=ORIENTED_EDGE('',*,*,#4117,.F.);
#5427=ORIENTED_EDGE('',*,*,#4119,.F.);
#5428=ORIENTED_EDGE('',*,*,#4120,.F.);
#5429=ORIENTED_EDGE('',*,*,#4121,.F.);
#5430=ORIENTED_EDGE('',*,*,#4122,.T.);
#5431=ORIENTED_EDGE('',*,*,#4122,.F.);
#5432=ORIENTED_EDGE('',*,*,#4123,.F.);
#5433=ORIENTED_EDGE('',*,*,#4124,.F.);
#5434=ORIENTED_EDGE('',*,*,#4125,.F.);
#5435=ORIENTED_EDGE('',*,*,#4126,.F.);
#5436=ORIENTED_EDGE('',*,*,#4127,.F.);
#5437=ORIENTED_EDGE('',*,*,#4128,.F.);
#5438=ORIENTED_EDGE('',*,*,#4129,.F.);
#5439=ORIENTED_EDGE('',*,*,#4130,.F.);
#5440=ORIENTED_EDGE('',*,*,#4116,.T.);
#5441=ORIENTED_EDGE('',*,*,#4131,.F.);
#5442=ORIENTED_EDGE('',*,*,#4121,.T.);
#5443=ORIENTED_EDGE('',*,*,#4132,.F.);
#5444=ORIENTED_EDGE('',*,*,#4133,.F.);
#5445=ORIENTED_EDGE('',*,*,#4123,.T.);
#5446=ORIENTED_EDGE('',*,*,#4134,.T.);
#5447=ORIENTED_EDGE('',*,*,#4135,.F.);
#5448=ORIENTED_EDGE('',*,*,#4132,.T.);
#5449=ORIENTED_EDGE('',*,*,#4120,.T.);
#5450=ORIENTED_EDGE('',*,*,#4119,.T.);
#5451=ORIENTED_EDGE('',*,*,#4130,.T.);
#5452=ORIENTED_EDGE('',*,*,#4136,.F.);
#5453=ORIENTED_EDGE('',*,*,#4134,.F.);
#5454=ORIENTED_EDGE('',*,*,#4137,.F.);
#5455=ORIENTED_EDGE('',*,*,#4138,.F.);
#5456=ORIENTED_EDGE('',*,*,#4139,.F.);
#5457=ORIENTED_EDGE('',*,*,#4127,.T.);
#5458=ORIENTED_EDGE('',*,*,#4139,.T.);
#5459=ORIENTED_EDGE('',*,*,#4140,.F.);
#5460=ORIENTED_EDGE('',*,*,#4141,.F.);
#5461=ORIENTED_EDGE('',*,*,#4128,.T.);
#5462=ORIENTED_EDGE('',*,*,#4142,.T.);
#5463=ORIENTED_EDGE('',*,*,#4143,.F.);
#5464=ORIENTED_EDGE('',*,*,#4140,.T.);
#5465=ORIENTED_EDGE('',*,*,#4138,.T.);
#5466=ORIENTED_EDGE('',*,*,#4118,.T.);
#5467=ORIENTED_EDGE('',*,*,#4137,.T.);
#5468=ORIENTED_EDGE('',*,*,#4126,.T.);
#5469=ORIENTED_EDGE('',*,*,#4144,.F.);
#5470=ORIENTED_EDGE('',*,*,#4142,.F.);
#5471=ORIENTED_EDGE('',*,*,#4145,.T.);
#5472=ORIENTED_EDGE('',*,*,#4146,.F.);
#5473=ORIENTED_EDGE('',*,*,#4145,.F.);
#5474=ORIENTED_EDGE('',*,*,#4147,.T.);
#5475=ORIENTED_EDGE('',*,*,#4124,.T.);
#5476=ORIENTED_EDGE('',*,*,#4133,.T.);
#5477=ORIENTED_EDGE('',*,*,#4135,.T.);
#5478=ORIENTED_EDGE('',*,*,#4136,.T.);
#5479=ORIENTED_EDGE('',*,*,#4129,.T.);
#5480=ORIENTED_EDGE('',*,*,#4141,.T.);
#5481=ORIENTED_EDGE('',*,*,#4143,.T.);
#5482=ORIENTED_EDGE('',*,*,#4144,.T.);
#5483=ORIENTED_EDGE('',*,*,#4125,.T.);
#5484=ORIENTED_EDGE('',*,*,#4147,.F.);
#5485=ORIENTED_EDGE('',*,*,#4148,.T.);
#5486=ORIENTED_EDGE('',*,*,#4149,.F.);
#5487=ORIENTED_EDGE('',*,*,#4148,.F.);
#5488=ORIENTED_EDGE('',*,*,#4150,.T.);
#5489=ORIENTED_EDGE('',*,*,#4146,.T.);
#5490=ORIENTED_EDGE('',*,*,#4150,.F.);
#5491=ORIENTED_EDGE('',*,*,#4131,.T.);
#5492=ORIENTED_EDGE('',*,*,#4151,.T.);
#5493=ORIENTED_EDGE('',*,*,#4152,.T.);
#5494=ORIENTED_EDGE('',*,*,#4151,.F.);
#5495=ORIENTED_EDGE('',*,*,#4153,.F.);
#5496=ORIENTED_EDGE('',*,*,#4154,.T.);
#5497=ORIENTED_EDGE('',*,*,#4149,.T.);
#5498=ORIENTED_EDGE('',*,*,#4154,.F.);
#5499=ORIENTED_EDGE('',*,*,#4153,.T.);
#5500=ORIENTED_EDGE('',*,*,#4152,.F.);
#5501=ORIENTED_EDGE('',*,*,#4155,.F.);
#5502=ORIENTED_EDGE('',*,*,#4156,.T.);
#5503=ORIENTED_EDGE('',*,*,#4157,.T.);
#5504=ORIENTED_EDGE('',*,*,#4156,.F.);
#5505=ORIENTED_EDGE('',*,*,#4158,.F.);
#5506=ORIENTED_EDGE('',*,*,#4159,.T.);
#5507=ORIENTED_EDGE('',*,*,#4160,.T.);
#5508=ORIENTED_EDGE('',*,*,#4159,.F.);
#5509=ORIENTED_EDGE('',*,*,#4158,.T.);
#5510=ORIENTED_EDGE('',*,*,#4155,.T.);
#5511=ORIENTED_EDGE('',*,*,#4160,.F.);
#5512=ORIENTED_EDGE('',*,*,#4157,.F.);
#5513=ORIENTED_EDGE('',*,*,#4161,.F.);
#5514=ORIENTED_EDGE('',*,*,#4162,.T.);
#5515=ORIENTED_EDGE('',*,*,#4163,.F.);
#5516=ORIENTED_EDGE('',*,*,#4164,.F.);
#5517=ORIENTED_EDGE('',*,*,#4165,.T.);
#5518=ORIENTED_EDGE('',*,*,#4166,.F.);
#5519=ORIENTED_EDGE('',*,*,#4167,.F.);
#5520=ORIENTED_EDGE('',*,*,#4165,.F.);
#5521=ORIENTED_EDGE('',*,*,#4168,.F.);
#5522=ORIENTED_EDGE('',*,*,#4169,.F.);
#5523=ORIENTED_EDGE('',*,*,#4162,.F.);
#5524=ORIENTED_EDGE('',*,*,#4170,.F.);
#5525=ORIENTED_EDGE('',*,*,#4168,.T.);
#5526=ORIENTED_EDGE('',*,*,#4164,.T.);
#5527=ORIENTED_EDGE('',*,*,#4171,.F.);
#5528=ORIENTED_EDGE('',*,*,#4172,.T.);
#5529=ORIENTED_EDGE('',*,*,#4173,.T.);
#5530=ORIENTED_EDGE('',*,*,#4172,.F.);
#5531=ORIENTED_EDGE('',*,*,#4169,.T.);
#5532=ORIENTED_EDGE('',*,*,#4170,.T.);
#5533=ORIENTED_EDGE('',*,*,#4163,.T.);
#5534=ORIENTED_EDGE('',*,*,#4161,.T.);
#5535=ORIENTED_EDGE('',*,*,#4174,.F.);
#5536=ORIENTED_EDGE('',*,*,#4175,.T.);
#5537=ORIENTED_EDGE('',*,*,#4176,.T.);
#5538=ORIENTED_EDGE('',*,*,#4175,.F.);
#5539=ORIENTED_EDGE('',*,*,#4166,.T.);
#5540=ORIENTED_EDGE('',*,*,#4167,.T.);
#5541=ORIENTED_EDGE('',*,*,#4174,.T.);
#5542=ORIENTED_EDGE('',*,*,#4171,.T.);
#5543=ORIENTED_EDGE('',*,*,#4176,.F.);
#5544=ORIENTED_EDGE('',*,*,#4173,.F.);
#5545=ORIENTED_EDGE('',*,*,#4177,.F.);
#5546=ORIENTED_EDGE('',*,*,#4178,.T.);
#5547=ORIENTED_EDGE('',*,*,#4179,.F.);
#5548=ORIENTED_EDGE('',*,*,#4178,.F.);
#5549=ORIENTED_EDGE('',*,*,#4177,.T.);
#5550=ORIENTED_EDGE('',*,*,#4180,.F.);
#5551=ORIENTED_EDGE('',*,*,#4181,.T.);
#5552=ORIENTED_EDGE('',*,*,#4182,.T.);
#5553=ORIENTED_EDGE('',*,*,#4181,.F.);
#5554=ORIENTED_EDGE('',*,*,#4182,.F.);
#5555=ORIENTED_EDGE('',*,*,#4183,.T.);
#5556=ORIENTED_EDGE('',*,*,#4184,.F.);
#5557=ORIENTED_EDGE('',*,*,#4185,.F.);
#5558=ORIENTED_EDGE('',*,*,#4186,.F.);
#5559=ORIENTED_EDGE('',*,*,#4183,.F.);
#5560=ORIENTED_EDGE('',*,*,#4187,.T.);
#5561=ORIENTED_EDGE('',*,*,#4185,.T.);
#5562=ORIENTED_EDGE('',*,*,#4187,.F.);
#5563=ORIENTED_EDGE('',*,*,#4186,.T.);
#5564=ORIENTED_EDGE('',*,*,#4188,.T.);
#5565=ORIENTED_EDGE('',*,*,#4189,.T.);
#5566=ORIENTED_EDGE('',*,*,#4188,.F.);
#5567=ORIENTED_EDGE('',*,*,#4190,.F.);
#5568=ORIENTED_EDGE('',*,*,#4191,.T.);
#5569=ORIENTED_EDGE('',*,*,#4184,.T.);
#5570=ORIENTED_EDGE('',*,*,#4191,.F.);
#5571=ORIENTED_EDGE('',*,*,#4190,.T.);
#5572=ORIENTED_EDGE('',*,*,#4179,.T.);
#5573=ORIENTED_EDGE('',*,*,#4189,.F.);
#5574=ORIENTED_EDGE('',*,*,#4180,.T.);
#5575=ORIENTED_EDGE('',*,*,#4192,.F.);
#5576=ORIENTED_EDGE('',*,*,#4193,.T.);
#5577=ORIENTED_EDGE('',*,*,#4194,.T.);
#5578=ORIENTED_EDGE('',*,*,#4193,.F.);
#5579=ORIENTED_EDGE('',*,*,#4195,.F.);
#5580=ORIENTED_EDGE('',*,*,#4196,.T.);
#5581=ORIENTED_EDGE('',*,*,#4197,.T.);
#5582=ORIENTED_EDGE('',*,*,#4196,.F.);
#5583=ORIENTED_EDGE('',*,*,#4195,.T.);
#5584=ORIENTED_EDGE('',*,*,#4192,.T.);
#5585=ORIENTED_EDGE('',*,*,#4197,.F.);
#5586=ORIENTED_EDGE('',*,*,#4194,.F.);
#5587=ORIENTED_EDGE('',*,*,#4198,.F.);
#5588=ORIENTED_EDGE('',*,*,#4199,.T.);
#5589=ORIENTED_EDGE('',*,*,#4200,.T.);
#5590=ORIENTED_EDGE('',*,*,#4199,.F.);
#5591=ORIENTED_EDGE('',*,*,#4201,.F.);
#5592=ORIENTED_EDGE('',*,*,#4202,.T.);
#5593=ORIENTED_EDGE('',*,*,#4203,.T.);
#5594=ORIENTED_EDGE('',*,*,#4202,.F.);
#5595=ORIENTED_EDGE('',*,*,#4201,.T.);
#5596=ORIENTED_EDGE('',*,*,#4198,.T.);
#5597=ORIENTED_EDGE('',*,*,#4203,.F.);
#5598=ORIENTED_EDGE('',*,*,#4200,.F.);
#5599=ORIENTED_EDGE('',*,*,#4204,.F.);
#5600=ORIENTED_EDGE('',*,*,#4205,.T.);
#5601=ORIENTED_EDGE('',*,*,#4206,.T.);
#5602=ORIENTED_EDGE('',*,*,#4205,.F.);
#5603=ORIENTED_EDGE('',*,*,#4207,.F.);
#5604=ORIENTED_EDGE('',*,*,#4208,.T.);
#5605=ORIENTED_EDGE('',*,*,#4209,.T.);
#5606=ORIENTED_EDGE('',*,*,#4208,.F.);
#5607=ORIENTED_EDGE('',*,*,#4207,.T.);
#5608=ORIENTED_EDGE('',*,*,#4204,.T.);
#5609=ORIENTED_EDGE('',*,*,#4209,.F.);
#5610=ORIENTED_EDGE('',*,*,#4206,.F.);
#5611=ORIENTED_EDGE('',*,*,#4210,.F.);
#5612=ORIENTED_EDGE('',*,*,#4211,.T.);
#5613=ORIENTED_EDGE('',*,*,#4212,.T.);
#5614=ORIENTED_EDGE('',*,*,#4211,.F.);
#5615=ORIENTED_EDGE('',*,*,#4213,.F.);
#5616=ORIENTED_EDGE('',*,*,#4214,.T.);
#5617=ORIENTED_EDGE('',*,*,#4215,.T.);
#5618=ORIENTED_EDGE('',*,*,#4214,.F.);
#5619=ORIENTED_EDGE('',*,*,#4213,.T.);
#5620=ORIENTED_EDGE('',*,*,#4210,.T.);
#5621=ORIENTED_EDGE('',*,*,#4215,.F.);
#5622=ORIENTED_EDGE('',*,*,#4212,.F.);
#5623=ORIENTED_EDGE('',*,*,#4216,.F.);
#5624=ORIENTED_EDGE('',*,*,#4217,.F.);
#5625=ORIENTED_EDGE('',*,*,#4218,.T.);
#5626=ORIENTED_EDGE('',*,*,#4219,.T.);
#5627=ORIENTED_EDGE('',*,*,#4220,.F.);
#5628=ORIENTED_EDGE('',*,*,#4221,.F.);
#5629=ORIENTED_EDGE('',*,*,#4222,.T.);
#5630=ORIENTED_EDGE('',*,*,#4223,.T.);
#5631=ORIENTED_EDGE('',*,*,#4218,.F.);
#5632=ORIENTED_EDGE('',*,*,#4224,.F.);
#5633=ORIENTED_EDGE('',*,*,#4225,.T.);
#5634=ORIENTED_EDGE('',*,*,#4226,.T.);
#5635=ORIENTED_EDGE('',*,*,#4222,.F.);
#5636=ORIENTED_EDGE('',*,*,#4227,.F.);
#5637=ORIENTED_EDGE('',*,*,#4228,.T.);
#5638=ORIENTED_EDGE('',*,*,#4229,.T.);
#5639=ORIENTED_EDGE('',*,*,#4225,.F.);
#5640=ORIENTED_EDGE('',*,*,#4230,.F.);
#5641=ORIENTED_EDGE('',*,*,#4231,.T.);
#5642=ORIENTED_EDGE('',*,*,#4232,.T.);
#5643=ORIENTED_EDGE('',*,*,#4228,.F.);
#5644=ORIENTED_EDGE('',*,*,#4233,.F.);
#5645=ORIENTED_EDGE('',*,*,#4220,.T.);
#5646=ORIENTED_EDGE('',*,*,#4234,.T.);
#5647=ORIENTED_EDGE('',*,*,#4231,.F.);
#5648=ORIENTED_EDGE('',*,*,#4234,.F.);
#5649=ORIENTED_EDGE('',*,*,#4219,.F.);
#5650=ORIENTED_EDGE('',*,*,#4223,.F.);
#5651=ORIENTED_EDGE('',*,*,#4226,.F.);
#5652=ORIENTED_EDGE('',*,*,#4229,.F.);
#5653=ORIENTED_EDGE('',*,*,#4232,.F.);
#5654=ORIENTED_EDGE('',*,*,#4235,.F.);
#5655=ORIENTED_EDGE('',*,*,#4217,.T.);
#5656=ORIENTED_EDGE('',*,*,#4233,.T.);
#5657=ORIENTED_EDGE('',*,*,#4230,.T.);
#5658=ORIENTED_EDGE('',*,*,#4227,.T.);
#5659=ORIENTED_EDGE('',*,*,#4224,.T.);
#5660=ORIENTED_EDGE('',*,*,#4221,.T.);
#5661=ORIENTED_EDGE('',*,*,#4236,.F.);
#5662=ORIENTED_EDGE('',*,*,#4237,.T.);
#5663=ORIENTED_EDGE('',*,*,#4235,.T.);
#5664=ORIENTED_EDGE('',*,*,#4237,.F.);
#5665=ORIENTED_EDGE('',*,*,#4216,.T.);
#5666=ORIENTED_EDGE('',*,*,#4238,.T.);
#5667=ORIENTED_EDGE('',*,*,#4236,.T.);
#5668=ORIENTED_EDGE('',*,*,#4238,.F.);
#5669=ORIENTED_EDGE('',*,*,#4239,.T.);
#5670=ORIENTED_EDGE('',*,*,#4240,.T.);
#5671=ORIENTED_EDGE('',*,*,#4241,.T.);
#5672=ORIENTED_EDGE('',*,*,#4242,.F.);
#5673=ORIENTED_EDGE('',*,*,#4243,.T.);
#5674=ORIENTED_EDGE('',*,*,#4244,.T.);
#5675=ORIENTED_EDGE('',*,*,#4245,.T.);
#5676=ORIENTED_EDGE('',*,*,#4240,.F.);
#5677=ORIENTED_EDGE('',*,*,#4246,.T.);
#5678=ORIENTED_EDGE('',*,*,#4247,.T.);
#5679=ORIENTED_EDGE('',*,*,#4248,.T.);
#5680=ORIENTED_EDGE('',*,*,#4244,.F.);
#5681=ORIENTED_EDGE('',*,*,#4249,.T.);
#5682=ORIENTED_EDGE('',*,*,#4250,.T.);
#5683=ORIENTED_EDGE('',*,*,#4251,.T.);
#5684=ORIENTED_EDGE('',*,*,#4247,.F.);
#5685=ORIENTED_EDGE('',*,*,#4252,.T.);
#5686=ORIENTED_EDGE('',*,*,#4253,.T.);
#5687=ORIENTED_EDGE('',*,*,#4254,.T.);
#5688=ORIENTED_EDGE('',*,*,#4250,.F.);
#5689=ORIENTED_EDGE('',*,*,#4255,.T.);
#5690=ORIENTED_EDGE('',*,*,#4242,.T.);
#5691=ORIENTED_EDGE('',*,*,#4256,.T.);
#5692=ORIENTED_EDGE('',*,*,#4253,.F.);
#5693=ORIENTED_EDGE('',*,*,#4255,.F.);
#5694=ORIENTED_EDGE('',*,*,#4252,.F.);
#5695=ORIENTED_EDGE('',*,*,#4249,.F.);
#5696=ORIENTED_EDGE('',*,*,#4246,.F.);
#5697=ORIENTED_EDGE('',*,*,#4243,.F.);
#5698=ORIENTED_EDGE('',*,*,#4239,.F.);
#5699=ORIENTED_EDGE('',*,*,#4256,.F.);
#5700=ORIENTED_EDGE('',*,*,#4241,.F.);
#5701=ORIENTED_EDGE('',*,*,#4245,.F.);
#5702=ORIENTED_EDGE('',*,*,#4248,.F.);
#5703=ORIENTED_EDGE('',*,*,#4251,.F.);
#5704=ORIENTED_EDGE('',*,*,#4254,.F.);
#5705=ORIENTED_EDGE('',*,*,#4257,.F.);
#5706=ORIENTED_EDGE('',*,*,#4258,.F.);
#5707=ORIENTED_EDGE('',*,*,#4259,.F.);
#5708=ORIENTED_EDGE('',*,*,#4260,.T.);
#5709=ORIENTED_EDGE('',*,*,#4258,.T.);
#5710=ORIENTED_EDGE('',*,*,#4260,.F.);
#5711=ORIENTED_EDGE('',*,*,#4261,.F.);
#5712=ORIENTED_EDGE('',*,*,#4262,.T.);
#5713=ORIENTED_EDGE('',*,*,#4259,.T.);
#5714=ORIENTED_EDGE('',*,*,#4262,.F.);
#5715=ORIENTED_EDGE('',*,*,#4263,.F.);
#5716=ORIENTED_EDGE('',*,*,#4264,.T.);
#5717=ORIENTED_EDGE('',*,*,#4261,.T.);
#5718=ORIENTED_EDGE('',*,*,#4264,.F.);
#5719=ORIENTED_EDGE('',*,*,#4263,.T.);
#5720=ORIENTED_EDGE('',*,*,#4265,.F.);
#5721=ORIENTED_EDGE('',*,*,#4266,.F.);
#5722=ORIENTED_EDGE('',*,*,#4267,.T.);
#5723=ORIENTED_EDGE('',*,*,#4265,.T.);
#5724=ORIENTED_EDGE('',*,*,#4267,.F.);
#5725=ORIENTED_EDGE('',*,*,#4257,.T.);
#5726=ORIENTED_EDGE('',*,*,#4268,.T.);
#5727=ORIENTED_EDGE('',*,*,#4266,.T.);
#5728=ORIENTED_EDGE('',*,*,#4268,.F.);
#5729=ORIENTED_EDGE('',*,*,#4269,.F.);
#5730=ORIENTED_EDGE('',*,*,#4270,.F.);
#5731=ORIENTED_EDGE('',*,*,#4271,.T.);
#5732=ORIENTED_EDGE('',*,*,#4269,.T.);
#5733=ORIENTED_EDGE('',*,*,#4271,.F.);
#5734=ORIENTED_EDGE('',*,*,#4272,.F.);
#5735=ORIENTED_EDGE('',*,*,#4273,.T.);
#5736=ORIENTED_EDGE('',*,*,#4270,.T.);
#5737=ORIENTED_EDGE('',*,*,#4273,.F.);
#5738=ORIENTED_EDGE('',*,*,#4274,.F.);
#5739=ORIENTED_EDGE('',*,*,#4275,.T.);
#5740=ORIENTED_EDGE('',*,*,#4272,.T.);
#5741=ORIENTED_EDGE('',*,*,#4275,.F.);
#5742=ORIENTED_EDGE('',*,*,#4274,.T.);
#5743=ORIENTED_EDGE('',*,*,#4276,.F.);
#5744=ORIENTED_EDGE('',*,*,#4277,.F.);
#5745=ORIENTED_EDGE('',*,*,#4278,.T.);
#5746=ORIENTED_EDGE('',*,*,#4276,.T.);
#5747=ORIENTED_EDGE('',*,*,#4278,.F.);
#5748=ORIENTED_EDGE('',*,*,#4279,.F.);
#5749=ORIENTED_EDGE('',*,*,#4280,.T.);
#5750=ORIENTED_EDGE('',*,*,#4277,.T.);
#5751=ORIENTED_EDGE('',*,*,#4280,.F.);
#5752=ORIENTED_EDGE('',*,*,#4281,.F.);
#5753=ORIENTED_EDGE('',*,*,#4282,.T.);
#5754=ORIENTED_EDGE('',*,*,#4279,.T.);
#5755=ORIENTED_EDGE('',*,*,#4282,.F.);
#5756=ORIENTED_EDGE('',*,*,#4281,.T.);
#5757=ORIENTED_EDGE('',*,*,#4283,.T.);
#5758=ORIENTED_EDGE('',*,*,#4284,.T.);
#5759=ORIENTED_EDGE('',*,*,#4285,.T.);
#5760=ORIENTED_EDGE('',*,*,#4286,.F.);
#5761=ORIENTED_EDGE('',*,*,#4287,.T.);
#5762=ORIENTED_EDGE('',*,*,#4288,.T.);
#5763=ORIENTED_EDGE('',*,*,#4289,.T.);
#5764=ORIENTED_EDGE('',*,*,#4284,.F.);
#5765=ORIENTED_EDGE('',*,*,#4290,.T.);
#5766=ORIENTED_EDGE('',*,*,#4291,.T.);
#5767=ORIENTED_EDGE('',*,*,#4292,.T.);
#5768=ORIENTED_EDGE('',*,*,#4288,.F.);
#5769=ORIENTED_EDGE('',*,*,#4293,.T.);
#5770=ORIENTED_EDGE('',*,*,#4294,.T.);
#5771=ORIENTED_EDGE('',*,*,#4295,.T.);
#5772=ORIENTED_EDGE('',*,*,#4291,.F.);
#5773=ORIENTED_EDGE('',*,*,#4296,.T.);
#5774=ORIENTED_EDGE('',*,*,#4297,.T.);
#5775=ORIENTED_EDGE('',*,*,#4298,.T.);
#5776=ORIENTED_EDGE('',*,*,#4294,.F.);
#5777=ORIENTED_EDGE('',*,*,#4299,.T.);
#5778=ORIENTED_EDGE('',*,*,#4286,.T.);
#5779=ORIENTED_EDGE('',*,*,#4300,.T.);
#5780=ORIENTED_EDGE('',*,*,#4297,.F.);
#5781=ORIENTED_EDGE('',*,*,#4299,.F.);
#5782=ORIENTED_EDGE('',*,*,#4296,.F.);
#5783=ORIENTED_EDGE('',*,*,#4293,.F.);
#5784=ORIENTED_EDGE('',*,*,#4290,.F.);
#5785=ORIENTED_EDGE('',*,*,#4287,.F.);
#5786=ORIENTED_EDGE('',*,*,#4283,.F.);
#5787=ORIENTED_EDGE('',*,*,#4300,.F.);
#5788=ORIENTED_EDGE('',*,*,#4285,.F.);
#5789=ORIENTED_EDGE('',*,*,#4289,.F.);
#5790=ORIENTED_EDGE('',*,*,#4292,.F.);
#5791=ORIENTED_EDGE('',*,*,#4295,.F.);
#5792=ORIENTED_EDGE('',*,*,#4298,.F.);
#5793=ORIENTED_EDGE('',*,*,#4301,.F.);
#5794=ORIENTED_EDGE('',*,*,#4302,.T.);
#5795=ORIENTED_EDGE('',*,*,#4303,.F.);
#5796=ORIENTED_EDGE('',*,*,#4302,.F.);
#5797=ORIENTED_EDGE('',*,*,#4304,.F.);
#5798=ORIENTED_EDGE('',*,*,#4305,.T.);
#5799=ORIENTED_EDGE('',*,*,#4306,.F.);
#5800=ORIENTED_EDGE('',*,*,#4305,.F.);
#5801=ORIENTED_EDGE('',*,*,#4307,.F.);
#5802=ORIENTED_EDGE('',*,*,#4308,.F.);
#5803=ORIENTED_EDGE('',*,*,#4309,.F.);
#5804=ORIENTED_EDGE('',*,*,#4310,.T.);
#5805=ORIENTED_EDGE('',*,*,#4307,.T.);
#5806=ORIENTED_EDGE('',*,*,#4311,.T.);
#5807=ORIENTED_EDGE('',*,*,#4312,.F.);
#5808=ORIENTED_EDGE('',*,*,#4313,.F.);
#5809=ORIENTED_EDGE('',*,*,#4310,.F.);
#5810=ORIENTED_EDGE('',*,*,#4314,.F.);
#5811=ORIENTED_EDGE('',*,*,#4315,.F.);
#5812=ORIENTED_EDGE('',*,*,#4311,.F.);
#5813=ORIENTED_EDGE('',*,*,#4301,.T.);
#5814=ORIENTED_EDGE('',*,*,#4304,.T.);
#5815=ORIENTED_EDGE('',*,*,#4309,.T.);
#5816=ORIENTED_EDGE('',*,*,#4316,.F.);
#5817=ORIENTED_EDGE('',*,*,#4317,.F.);
#5818=ORIENTED_EDGE('',*,*,#4314,.T.);
#5819=ORIENTED_EDGE('',*,*,#4312,.T.);
#5820=ORIENTED_EDGE('',*,*,#4315,.T.);
#5821=ORIENTED_EDGE('',*,*,#4317,.T.);
#5822=ORIENTED_EDGE('',*,*,#4318,.F.);
#5823=ORIENTED_EDGE('',*,*,#4313,.T.);
#5824=ORIENTED_EDGE('',*,*,#4318,.T.);
#5825=ORIENTED_EDGE('',*,*,#4316,.T.);
#5826=ORIENTED_EDGE('',*,*,#4308,.T.);
#5827=ORIENTED_EDGE('',*,*,#4303,.T.);
#5828=ORIENTED_EDGE('',*,*,#4306,.T.);
#5829=ORIENTED_EDGE('',*,*,#4319,.F.);
#5830=ORIENTED_EDGE('',*,*,#4320,.T.);
#5831=ORIENTED_EDGE('',*,*,#4321,.T.);
#5832=ORIENTED_EDGE('',*,*,#4320,.F.);
#5833=ORIENTED_EDGE('',*,*,#4322,.F.);
#5834=ORIENTED_EDGE('',*,*,#4323,.T.);
#5835=ORIENTED_EDGE('',*,*,#4324,.T.);
#5836=ORIENTED_EDGE('',*,*,#4323,.F.);
#5837=ORIENTED_EDGE('',*,*,#4322,.T.);
#5838=ORIENTED_EDGE('',*,*,#4319,.T.);
#5839=ORIENTED_EDGE('',*,*,#4324,.F.);
#5840=ORIENTED_EDGE('',*,*,#4321,.F.);
#5841=ORIENTED_EDGE('',*,*,#4325,.F.);
#5842=ORIENTED_EDGE('',*,*,#4326,.T.);
#5843=ORIENTED_EDGE('',*,*,#4327,.T.);
#5844=ORIENTED_EDGE('',*,*,#4326,.F.);
#5845=ORIENTED_EDGE('',*,*,#4328,.F.);
#5846=ORIENTED_EDGE('',*,*,#4329,.T.);
#5847=ORIENTED_EDGE('',*,*,#4330,.T.);
#5848=ORIENTED_EDGE('',*,*,#4329,.F.);
#5849=ORIENTED_EDGE('',*,*,#4328,.T.);
#5850=ORIENTED_EDGE('',*,*,#4325,.T.);
#5851=ORIENTED_EDGE('',*,*,#4330,.F.);
#5852=ORIENTED_EDGE('',*,*,#4327,.F.);
#5853=ORIENTED_EDGE('',*,*,#4331,.F.);
#5854=ORIENTED_EDGE('',*,*,#4332,.T.);
#5855=ORIENTED_EDGE('',*,*,#4333,.T.);
#5856=ORIENTED_EDGE('',*,*,#4332,.F.);
#5857=ORIENTED_EDGE('',*,*,#4333,.F.);
#5858=ORIENTED_EDGE('',*,*,#4334,.F.);
#5859=ORIENTED_EDGE('',*,*,#4335,.F.);
#5860=ORIENTED_EDGE('',*,*,#4336,.F.);
#5861=ORIENTED_EDGE('',*,*,#4337,.F.);
#5862=ORIENTED_EDGE('',*,*,#4331,.T.);
#5863=ORIENTED_EDGE('',*,*,#4336,.T.);
#5864=ORIENTED_EDGE('',*,*,#4338,.T.);
#5865=ORIENTED_EDGE('',*,*,#4339,.F.);
#5866=ORIENTED_EDGE('',*,*,#4340,.F.);
#5867=ORIENTED_EDGE('',*,*,#4341,.T.);
#5868=ORIENTED_EDGE('',*,*,#4342,.F.);
#5869=ORIENTED_EDGE('',*,*,#4335,.T.);
#5870=ORIENTED_EDGE('',*,*,#4343,.F.);
#5871=ORIENTED_EDGE('',*,*,#4344,.F.);
#5872=ORIENTED_EDGE('',*,*,#4338,.F.);
#5873=ORIENTED_EDGE('',*,*,#4334,.T.);
#5874=ORIENTED_EDGE('',*,*,#4345,.F.);
#5875=ORIENTED_EDGE('',*,*,#4346,.F.);
#5876=ORIENTED_EDGE('',*,*,#4347,.F.);
#5877=ORIENTED_EDGE('',*,*,#4348,.F.);
#5878=ORIENTED_EDGE('',*,*,#4343,.T.);
#5879=ORIENTED_EDGE('',*,*,#4349,.F.);
#5880=ORIENTED_EDGE('',*,*,#4350,.F.);
#5881=ORIENTED_EDGE('',*,*,#4341,.F.);
#5882=ORIENTED_EDGE('',*,*,#4351,.F.);
#5883=ORIENTED_EDGE('',*,*,#4352,.F.);
#5884=ORIENTED_EDGE('',*,*,#4346,.T.);
#5885=ORIENTED_EDGE('',*,*,#4353,.F.);
#5886=ORIENTED_EDGE('',*,*,#4354,.F.);
#5887=ORIENTED_EDGE('',*,*,#4337,.T.);
#5888=ORIENTED_EDGE('',*,*,#4342,.T.);
#5889=ORIENTED_EDGE('',*,*,#4350,.T.);
#5890=ORIENTED_EDGE('',*,*,#4355,.F.);
#5891=ORIENTED_EDGE('',*,*,#4353,.T.);
#5892=ORIENTED_EDGE('',*,*,#4345,.T.);
#5893=ORIENTED_EDGE('',*,*,#4356,.F.);
#5894=ORIENTED_EDGE('',*,*,#4357,.T.);
#5895=ORIENTED_EDGE('',*,*,#4355,.T.);
#5896=ORIENTED_EDGE('',*,*,#4349,.T.);
#5897=ORIENTED_EDGE('',*,*,#4358,.T.);
#5898=ORIENTED_EDGE('',*,*,#4354,.T.);
#5899=ORIENTED_EDGE('',*,*,#4357,.F.);
#5900=ORIENTED_EDGE('',*,*,#4347,.T.);
#5901=ORIENTED_EDGE('',*,*,#4352,.T.);
#5902=ORIENTED_EDGE('',*,*,#4358,.F.);
#5903=ORIENTED_EDGE('',*,*,#4351,.T.);
#5904=ORIENTED_EDGE('',*,*,#4340,.T.);
#5905=ORIENTED_EDGE('',*,*,#4359,.T.);
#5906=ORIENTED_EDGE('',*,*,#4360,.T.);
#5907=ORIENTED_EDGE('',*,*,#4348,.T.);
#5908=ORIENTED_EDGE('',*,*,#4360,.F.);
#5909=ORIENTED_EDGE('',*,*,#4361,.T.);
#5910=ORIENTED_EDGE('',*,*,#4362,.T.);
#5911=ORIENTED_EDGE('',*,*,#4361,.F.);
#5912=ORIENTED_EDGE('',*,*,#4359,.F.);
#5913=ORIENTED_EDGE('',*,*,#4339,.T.);
#5914=ORIENTED_EDGE('',*,*,#4344,.T.);
#5915=ORIENTED_EDGE('',*,*,#4362,.F.);
#5916=ORIENTED_EDGE('',*,*,#4356,.T.);
#5917=ORIENTED_EDGE('',*,*,#4363,.F.);
#5918=ORIENTED_EDGE('',*,*,#4364,.T.);
#5919=ORIENTED_EDGE('',*,*,#4365,.F.);
#5920=ORIENTED_EDGE('',*,*,#4366,.F.);
#5921=ORIENTED_EDGE('',*,*,#4367,.T.);
#5922=ORIENTED_EDGE('',*,*,#4368,.F.);
#5923=ORIENTED_EDGE('',*,*,#4367,.F.);
#5924=ORIENTED_EDGE('',*,*,#4369,.F.);
#5925=ORIENTED_EDGE('',*,*,#4370,.F.);
#5926=ORIENTED_EDGE('',*,*,#4364,.F.);
#5927=ORIENTED_EDGE('',*,*,#4371,.F.);
#5928=ORIENTED_EDGE('',*,*,#4369,.T.);
#5929=ORIENTED_EDGE('',*,*,#4366,.T.);
#5930=ORIENTED_EDGE('',*,*,#4372,.F.);
#5931=ORIENTED_EDGE('',*,*,#4373,.T.);
#5932=ORIENTED_EDGE('',*,*,#4374,.F.);
#5933=ORIENTED_EDGE('',*,*,#4373,.F.);
#5934=ORIENTED_EDGE('',*,*,#4370,.T.);
#5935=ORIENTED_EDGE('',*,*,#4371,.T.);
#5936=ORIENTED_EDGE('',*,*,#4365,.T.);
#5937=ORIENTED_EDGE('',*,*,#4363,.T.);
#5938=ORIENTED_EDGE('',*,*,#4375,.T.);
#5939=ORIENTED_EDGE('',*,*,#4376,.T.);
#5940=ORIENTED_EDGE('',*,*,#4377,.F.);
#5941=ORIENTED_EDGE('',*,*,#4378,.F.);
#5942=ORIENTED_EDGE('',*,*,#4372,.T.);
#5943=ORIENTED_EDGE('',*,*,#4379,.T.);
#5944=ORIENTED_EDGE('',*,*,#4380,.T.);
#5945=ORIENTED_EDGE('',*,*,#4378,.T.);
#5946=ORIENTED_EDGE('',*,*,#4381,.F.);
#5947=ORIENTED_EDGE('',*,*,#4382,.T.);
#5948=ORIENTED_EDGE('',*,*,#4381,.T.);
#5949=ORIENTED_EDGE('',*,*,#4377,.T.);
#5950=ORIENTED_EDGE('',*,*,#4383,.T.);
#5951=ORIENTED_EDGE('',*,*,#4384,.T.);
#5952=ORIENTED_EDGE('',*,*,#4385,.F.);
#5953=ORIENTED_EDGE('',*,*,#4375,.F.);
#5954=ORIENTED_EDGE('',*,*,#4380,.F.);
#5955=ORIENTED_EDGE('',*,*,#4386,.T.);
#5956=ORIENTED_EDGE('',*,*,#4383,.F.);
#5957=ORIENTED_EDGE('',*,*,#4376,.F.);
#5958=ORIENTED_EDGE('',*,*,#4385,.T.);
#5959=ORIENTED_EDGE('',*,*,#4368,.T.);
#5960=ORIENTED_EDGE('',*,*,#4379,.F.);
#5961=ORIENTED_EDGE('',*,*,#4382,.F.);
#5962=ORIENTED_EDGE('',*,*,#4386,.F.);
#5963=ORIENTED_EDGE('',*,*,#4384,.F.);
#5964=ORIENTED_EDGE('',*,*,#4374,.T.);
#5965=ORIENTED_EDGE('',*,*,#4387,.T.);
#5966=ORIENTED_EDGE('',*,*,#4388,.F.);
#5967=ORIENTED_EDGE('',*,*,#4387,.F.);
#5968=ORIENTED_EDGE('',*,*,#4389,.T.);
#5969=ORIENTED_EDGE('',*,*,#4390,.T.);
#5970=ORIENTED_EDGE('',*,*,#4389,.F.);
#5971=ORIENTED_EDGE('',*,*,#4390,.F.);
#5972=ORIENTED_EDGE('',*,*,#4391,.F.);
#5973=ORIENTED_EDGE('',*,*,#4392,.T.);
#5974=ORIENTED_EDGE('',*,*,#4388,.T.);
#5975=ORIENTED_EDGE('',*,*,#4392,.F.);
#5976=ORIENTED_EDGE('',*,*,#4391,.T.);
#5977=ORIENTED_EDGE('',*,*,#4393,.F.);
#5978=ORIENTED_EDGE('',*,*,#4394,.T.);
#5979=ORIENTED_EDGE('',*,*,#4395,.T.);
#5980=ORIENTED_EDGE('',*,*,#4394,.F.);
#5981=ORIENTED_EDGE('',*,*,#4393,.T.);
#5982=ORIENTED_EDGE('',*,*,#4395,.F.);
#5983=ORIENTED_EDGE('',*,*,#4396,.F.);
#5984=ORIENTED_EDGE('',*,*,#4397,.T.);
#5985=ORIENTED_EDGE('',*,*,#4398,.T.);
#5986=ORIENTED_EDGE('',*,*,#4399,.F.);
#5987=ORIENTED_EDGE('',*,*,#4400,.F.);
#5988=ORIENTED_EDGE('',*,*,#4401,.T.);
#5989=ORIENTED_EDGE('',*,*,#4402,.T.);
#5990=ORIENTED_EDGE('',*,*,#4397,.F.);
#5991=ORIENTED_EDGE('',*,*,#4403,.F.);
#5992=ORIENTED_EDGE('',*,*,#4404,.T.);
#5993=ORIENTED_EDGE('',*,*,#4405,.T.);
#5994=ORIENTED_EDGE('',*,*,#4401,.F.);
#5995=ORIENTED_EDGE('',*,*,#4406,.F.);
#5996=ORIENTED_EDGE('',*,*,#4407,.T.);
#5997=ORIENTED_EDGE('',*,*,#4408,.T.);
#5998=ORIENTED_EDGE('',*,*,#4404,.F.);
#5999=ORIENTED_EDGE('',*,*,#4409,.F.);
#6000=ORIENTED_EDGE('',*,*,#4410,.T.);
#6001=ORIENTED_EDGE('',*,*,#4411,.T.);
#6002=ORIENTED_EDGE('',*,*,#4407,.F.);
#6003=ORIENTED_EDGE('',*,*,#4412,.F.);
#6004=ORIENTED_EDGE('',*,*,#4399,.T.);
#6005=ORIENTED_EDGE('',*,*,#4413,.T.);
#6006=ORIENTED_EDGE('',*,*,#4410,.F.);
#6007=ORIENTED_EDGE('',*,*,#4413,.F.);
#6008=ORIENTED_EDGE('',*,*,#4398,.F.);
#6009=ORIENTED_EDGE('',*,*,#4402,.F.);
#6010=ORIENTED_EDGE('',*,*,#4405,.F.);
#6011=ORIENTED_EDGE('',*,*,#4408,.F.);
#6012=ORIENTED_EDGE('',*,*,#4411,.F.);
#6013=ORIENTED_EDGE('',*,*,#4414,.F.);
#6014=ORIENTED_EDGE('',*,*,#4396,.T.);
#6015=ORIENTED_EDGE('',*,*,#4412,.T.);
#6016=ORIENTED_EDGE('',*,*,#4409,.T.);
#6017=ORIENTED_EDGE('',*,*,#4406,.T.);
#6018=ORIENTED_EDGE('',*,*,#4403,.T.);
#6019=ORIENTED_EDGE('',*,*,#4400,.T.);
#6020=ORIENTED_EDGE('',*,*,#4415,.F.);
#6021=ORIENTED_EDGE('',*,*,#4416,.T.);
#6022=ORIENTED_EDGE('',*,*,#4414,.T.);
#6023=ORIENTED_EDGE('',*,*,#4416,.F.);
#6024=ORIENTED_EDGE('',*,*,#4417,.F.);
#6025=ORIENTED_EDGE('',*,*,#4418,.T.);
#6026=ORIENTED_EDGE('',*,*,#4415,.T.);
#6027=ORIENTED_EDGE('',*,*,#4418,.F.);
#6028=ORIENTED_EDGE('',*,*,#4419,.F.);
#6029=ORIENTED_EDGE('',*,*,#4420,.T.);
#6030=ORIENTED_EDGE('',*,*,#4417,.T.);
#6031=ORIENTED_EDGE('',*,*,#4420,.F.);
#6032=ORIENTED_EDGE('',*,*,#4419,.T.);
#6033=CYLINDRICAL_SURFACE('',#7042,0.225);
#6034=CYLINDRICAL_SURFACE('',#7045,0.225);
#6035=CYLINDRICAL_SURFACE('',#7048,0.225);
#6036=CYLINDRICAL_SURFACE('',#7051,0.225);
#6037=CYLINDRICAL_SURFACE('',#7054,0.21);
#6038=CYLINDRICAL_SURFACE('',#7057,0.210000000000001);
#6039=CYLINDRICAL_SURFACE('',#7060,0.210000000000001);
#6040=CYLINDRICAL_SURFACE('',#7063,0.21);
#6041=CYLINDRICAL_SURFACE('',#7087,0.225);
#6042=CYLINDRICAL_SURFACE('',#7090,0.165);
#6043=CYLINDRICAL_SURFACE('',#7094,0.165);
#6044=CYLINDRICAL_SURFACE('',#7098,0.165);
#6045=CYLINDRICAL_SURFACE('',#7102,0.165);
#6046=CYLINDRICAL_SURFACE('',#7106,0.165);
#6047=CYLINDRICAL_SURFACE('',#7109,0.165);
#6048=CYLINDRICAL_SURFACE('',#7112,0.165);
#6049=CYLINDRICAL_SURFACE('',#7115,0.165);
#6050=CYLINDRICAL_SURFACE('',#7118,0.275);
#6051=CYLINDRICAL_SURFACE('',#7121,0.275);
#6052=CYLINDRICAL_SURFACE('',#7124,0.275);
#6053=CYLINDRICAL_SURFACE('',#7127,0.275);
#6054=CYLINDRICAL_SURFACE('',#7130,1.05);
#6055=CYLINDRICAL_SURFACE('',#7135,0.625);
#6056=CYLINDRICAL_SURFACE('',#7137,1.5);
#6057=CYLINDRICAL_SURFACE('',#7140,2.);
#6058=CYLINDRICAL_SURFACE('',#7152,2.2);
#6059=CYLINDRICAL_SURFACE('',#7162,0.225);
#6060=CYLINDRICAL_SURFACE('',#7165,0.225);
#6061=CYLINDRICAL_SURFACE('',#7168,0.225);
#6062=CYLINDRICAL_SURFACE('',#7171,0.225);
#6063=CYLINDRICAL_SURFACE('',#7174,1.49);
#6064=CYLINDRICAL_SURFACE('',#7179,0.71);
#6065=CYLINDRICAL_SURFACE('',#7181,2.2);
#6066=CYLINDRICAL_SURFACE('',#7187,0.225);
#6067=CYLINDRICAL_SURFACE('',#7190,0.225);
#6068=CYLINDRICAL_SURFACE('',#7193,0.225);
#6069=CYLINDRICAL_SURFACE('',#7196,0.225);
#6070=CYLINDRICAL_SURFACE('',#7199,1.49);
#6071=CYLINDRICAL_SURFACE('',#7204,0.71);
#6072=CYLINDRICAL_SURFACE('',#7206,2.2);
#6073=CYLINDRICAL_SURFACE('',#7212,0.375);
#6074=CYLINDRICAL_SURFACE('',#7217,0.375);
#6075=CYLINDRICAL_SURFACE('',#7222,0.375);
#6076=CYLINDRICAL_SURFACE('',#7227,0.375);
#6077=CYLINDRICAL_SURFACE('',#7232,0.225);
#6078=CYLINDRICAL_SURFACE('',#7234,0.225);
#6079=CYLINDRICAL_SURFACE('',#7236,0.225);
#6080=CYLINDRICAL_SURFACE('',#7238,0.225);
#6081=CYLINDRICAL_SURFACE('',#7240,1.04);
#6082=CYLINDRICAL_SURFACE('',#7245,0.625);
#6083=CYLINDRICAL_SURFACE('',#7247,2.);
#6084=CYLINDRICAL_SURFACE('',#7260,0.165);
#6085=CYLINDRICAL_SURFACE('',#7264,0.165);
#6086=CYLINDRICAL_SURFACE('',#7275,0.165);
#6087=CYLINDRICAL_SURFACE('',#7279,0.165);
#6088=CYLINDRICAL_SURFACE('',#7290,0.165);
#6089=CYLINDRICAL_SURFACE('',#7297,0.5);
#6090=CYLINDRICAL_SURFACE('',#7300,0.3);
#6091=CYLINDRICAL_SURFACE('',#7318,0.425);
#6092=CYLINDRICAL_SURFACE('',#7326,0.24505);
#6093=CYLINDRICAL_SURFACE('',#7335,0.976185);
#6094=CYLINDRICAL_SURFACE('',#7337,0.5);
#6095=CYLINDRICAL_SURFACE('',#7343,0.976185);
#6096=CYLINDRICAL_SURFACE('',#7355,1.023815);
#6097=CYLINDRICAL_SURFACE('',#7362,1.5);
#6098=CYLINDRICAL_SURFACE('',#7367,1.023815);
#6099=CYLINDRICAL_SURFACE('',#7389,1.019052);
#6100=CYLINDRICAL_SURFACE('',#7429,0.980948);
#6101=CYLINDRICAL_SURFACE('',#7443,1.013815);
#6102=CYLINDRICAL_SURFACE('',#7447,0.991185);
#6103=CYLINDRICAL_SURFACE('',#7451,1.013815);
#6104=CYLINDRICAL_SURFACE('',#7455,0.991185);
#6105=CYLINDRICAL_SURFACE('',#7473,1.05);
#6106=CYLINDRICAL_SURFACE('',#7477,1.);
#6107=CYLINDRICAL_SURFACE('',#7481,1.05);
#6108=CYLINDRICAL_SURFACE('',#7485,1.);
#6109=CYLINDRICAL_SURFACE('',#7489,1.05);
#6110=CYLINDRICAL_SURFACE('',#7493,0.9);
#6111=CYLINDRICAL_SURFACE('',#7506,0.895);
#6112=CYLINDRICAL_SURFACE('',#7510,0.605);
#6113=CYLINDRICAL_SURFACE('',#7525,0.2);
#6114=CYLINDRICAL_SURFACE('',#7532,0.35);
#6115=CYLINDRICAL_SURFACE('',#7540,0.1954);
#6116=CYLINDRICAL_SURFACE('',#7545,0.305);
#6117=CYLINDRICAL_SURFACE('',#7548,0.8);
#6118=CYLINDRICAL_SURFACE('',#7561,0.7);
#6119=CYLINDRICAL_SURFACE('',#7570,1.);
#6120=CYLINDRICAL_SURFACE('',#7574,0.7);
#6121=CYLINDRICAL_SURFACE('',#7575,0.5);
#6122=CYLINDRICAL_SURFACE('',#7577,0.5);
#6123=CYLINDRICAL_SURFACE('',#7582,0.505);
#6124=CYLINDRICAL_SURFACE('',#7585,0.7);
#6125=CYLINDRICAL_SURFACE('',#7593,0.164999999999999);
#6126=CYLINDRICAL_SURFACE('',#7597,0.505);
#6127=CYLINDRICAL_SURFACE('',#7600,0.9);
#6128=CYLINDRICAL_SURFACE('',#7606,0.165);
#6129=CYLINDRICAL_SURFACE('',#7610,0.165);
#6130=CYLINDRICAL_SURFACE('',#7620,0.7);
#6131=CYLINDRICAL_SURFACE('',#7621,0.3);
#6132=CYLINDRICAL_SURFACE('',#7623,0.3);
#6133=CYLINDRICAL_SURFACE('',#7628,0.305);
#6134=CYLINDRICAL_SURFACE('',#7631,0.5);
#6135=CYLINDRICAL_SURFACE('',#7637,0.305);
#6136=CYLINDRICAL_SURFACE('',#7640,0.5);
#6137=CYLINDRICAL_SURFACE('',#7646,0.225);
#6138=CYLINDRICAL_SURFACE('',#7649,0.5);
#6139=CYLINDRICAL_SURFACE('',#7655,0.225);
#6140=CYLINDRICAL_SURFACE('',#7658,0.5);
#6141=CYLINDRICAL_SURFACE('',#7677,0.1954);
#6142=CYLINDRICAL_SURFACE('',#7693,0.35);
#6143=CYLINDRICAL_SURFACE('',#7701,0.1954);
#6144=CYLINDRICAL_SURFACE('',#7707,0.35);
#6145=CYLINDRICAL_SURFACE('',#7715,0.1954);
#6146=CYLINDRICAL_SURFACE('',#7775,0.5);
#6147=CYLINDRICAL_SURFACE('',#7778,0.5);
#6148=CYLINDRICAL_SURFACE('',#7781,0.8);
#6149=CYLINDRICAL_SURFACE('',#7788,0.8);
#6150=CYLINDRICAL_SURFACE('',#7792,0.305);
#6151=CYLINDRICAL_SURFACE('',#7795,0.5);
#6152=CYLINDRICAL_SURFACE('',#7801,0.305);
#6153=CYLINDRICAL_SURFACE('',#7804,0.5);
#6154=CYLINDRICAL_SURFACE('',#7814,0.305);
#6155=CYLINDRICAL_SURFACE('',#7827,0.6);
#6156=CYLINDRICAL_SURFACE('',#7833,1.2);
#6157=CYLINDRICAL_SURFACE('',#7839,0.165);
#6158=CYLINDRICAL_SURFACE('',#7844,0.305);
#6159=CYLINDRICAL_SURFACE('',#7857,0.5);
#6160=CYLINDRICAL_SURFACE('',#7860,0.3);
#6161=CYLINDRICAL_SURFACE('',#7864,1.);
#6162=CYLINDRICAL_SURFACE('',#7881,0.1954);
#6163=ADVANCED_FACE('',(#888),#6033,.F.);
#6164=ADVANCED_FACE('',(#889),#6034,.F.);
#6165=ADVANCED_FACE('',(#890),#6035,.F.);
#6166=ADVANCED_FACE('',(#891),#6036,.F.);
#6167=ADVANCED_FACE('',(#892),#6037,.F.);
#6168=ADVANCED_FACE('',(#893),#6038,.F.);
#6169=ADVANCED_FACE('',(#894),#6039,.F.);
#6170=ADVANCED_FACE('',(#895),#6040,.F.);
#6171=ADVANCED_FACE('',(#896),#651,.T.);
#6172=ADVANCED_FACE('',(#897),#652,.T.);
#6173=ADVANCED_FACE('',(#898),#653,.T.);
#6174=ADVANCED_FACE('',(#899),#654,.T.);
#6175=ADVANCED_FACE('',(#900,#500,#501,#502,#503,#504,#505,#506,#507),#655,
 .T.);
#6176=ADVANCED_FACE('',(#901,#508,#509,#510,#511,#512,#513,#514,#515),#656,
 .F.);
#6177=ADVANCED_FACE('',(#902),#657,.T.);
#6178=ADVANCED_FACE('',(#903),#658,.T.);
#6179=ADVANCED_FACE('',(#904),#659,.T.);
#6180=ADVANCED_FACE('',(#905),#660,.T.);
#6181=ADVANCED_FACE('',(#906),#661,.T.);
#6182=ADVANCED_FACE('',(#907),#662,.F.);
#6183=ADVANCED_FACE('',(#908),#663,.T.);
#6184=ADVANCED_FACE('',(#909),#664,.T.);
#6185=ADVANCED_FACE('',(#910),#665,.T.);
#6186=ADVANCED_FACE('',(#911),#666,.T.);
#6187=ADVANCED_FACE('',(#912),#667,.T.);
#6188=ADVANCED_FACE('',(#913),#668,.F.);
#6189=ADVANCED_FACE('',(#914),#6041,.F.);
#6190=ADVANCED_FACE('',(#915),#6042,.F.);
#6191=ADVANCED_FACE('',(#916),#669,.T.);
#6192=ADVANCED_FACE('',(#917),#6043,.F.);
#6193=ADVANCED_FACE('',(#918),#670,.T.);
#6194=ADVANCED_FACE('',(#919),#6044,.F.);
#6195=ADVANCED_FACE('',(#920),#671,.T.);
#6196=ADVANCED_FACE('',(#921),#6045,.F.);
#6197=ADVANCED_FACE('',(#922),#672,.T.);
#6198=ADVANCED_FACE('',(#923),#6046,.F.);
#6199=ADVANCED_FACE('',(#924),#6047,.F.);
#6200=ADVANCED_FACE('',(#925),#6048,.F.);
#6201=ADVANCED_FACE('',(#926),#6049,.F.);
#6202=ADVANCED_FACE('',(#927),#6050,.F.);
#6203=ADVANCED_FACE('',(#928),#6051,.F.);
#6204=ADVANCED_FACE('',(#929),#6052,.F.);
#6205=ADVANCED_FACE('',(#930),#6053,.F.);
#6206=ADVANCED_FACE('',(#931),#6054,.F.);
#6207=ADVANCED_FACE('',(#932,#516),#673,.T.);
#6208=ADVANCED_FACE('',(#933),#6055,.F.);
#6209=ADVANCED_FACE('',(#934),#6056,.F.);
#6210=ADVANCED_FACE('',(#935),#6057,.T.);
#6211=ADVANCED_FACE('',(#936,#517,#518,#519,#520,#521,#522),#674,.T.);
#6212=ADVANCED_FACE('',(#937,#523,#524,#525,#526,#527),#675,.T.);
#6213=ADVANCED_FACE('',(#938,#528,#529,#530,#531,#532),#676,.T.);
#6214=ADVANCED_FACE('',(#939),#677,.T.);
#6215=ADVANCED_FACE('',(#940),#678,.T.);
#6216=ADVANCED_FACE('',(#941),#679,.T.);
#6217=ADVANCED_FACE('',(#942),#680,.T.);
#6218=ADVANCED_FACE('',(#943),#681,.T.);
#6219=ADVANCED_FACE('',(#944),#6058,.T.);
#6220=ADVANCED_FACE('',(#945,#533,#534,#535,#536,#537,#538),#682,.T.);
#6221=ADVANCED_FACE('',(#946),#683,.T.);
#6222=ADVANCED_FACE('',(#947,#539),#684,.T.);
#6223=ADVANCED_FACE('',(#948),#685,.T.);
#6224=ADVANCED_FACE('',(#949),#686,.T.);
#6225=ADVANCED_FACE('',(#950),#687,.T.);
#6226=ADVANCED_FACE('',(#951,#540,#541,#542,#543),#688,.F.);
#6227=ADVANCED_FACE('',(#952),#6059,.F.);
#6228=ADVANCED_FACE('',(#953),#6060,.F.);
#6229=ADVANCED_FACE('',(#954),#6061,.F.);
#6230=ADVANCED_FACE('',(#955),#6062,.F.);
#6231=ADVANCED_FACE('',(#956),#6063,.T.);
#6232=ADVANCED_FACE('',(#957,#544),#689,.T.);
#6233=ADVANCED_FACE('',(#958),#6064,.F.);
#6234=ADVANCED_FACE('',(#959),#6065,.T.);
#6235=ADVANCED_FACE('',(#960,#545,#546,#547,#548,#549),#690,.T.);
#6236=ADVANCED_FACE('',(#961,#550,#551,#552,#553,#554),#691,.F.);
#6237=ADVANCED_FACE('',(#962),#6066,.F.);
#6238=ADVANCED_FACE('',(#963),#6067,.F.);
#6239=ADVANCED_FACE('',(#964),#6068,.F.);
#6240=ADVANCED_FACE('',(#965),#6069,.F.);
#6241=ADVANCED_FACE('',(#966),#6070,.T.);
#6242=ADVANCED_FACE('',(#967,#555),#692,.F.);
#6243=ADVANCED_FACE('',(#968),#6071,.F.);
#6244=ADVANCED_FACE('',(#969),#6072,.T.);
#6245=ADVANCED_FACE('',(#970,#556,#557,#558,#559,#560),#693,.T.);
#6246=ADVANCED_FACE('',(#971,#561,#562,#563,#564,#565),#694,.F.);
#6247=ADVANCED_FACE('',(#972),#6073,.F.);
#6248=ADVANCED_FACE('',(#973,#566),#695,.T.);
#6249=ADVANCED_FACE('',(#974),#6074,.F.);
#6250=ADVANCED_FACE('',(#975,#567),#696,.T.);
#6251=ADVANCED_FACE('',(#976),#6075,.F.);
#6252=ADVANCED_FACE('',(#977,#568),#697,.T.);
#6253=ADVANCED_FACE('',(#978),#6076,.F.);
#6254=ADVANCED_FACE('',(#979,#569),#698,.T.);
#6255=ADVANCED_FACE('',(#980),#6077,.F.);
#6256=ADVANCED_FACE('',(#981),#6078,.F.);
#6257=ADVANCED_FACE('',(#982),#6079,.F.);
#6258=ADVANCED_FACE('',(#983),#6080,.F.);
#6259=ADVANCED_FACE('',(#984),#6081,.T.);
#6260=ADVANCED_FACE('',(#985,#570),#699,.F.);
#6261=ADVANCED_FACE('',(#986),#6082,.F.);
#6262=ADVANCED_FACE('',(#987),#6083,.T.);
#6263=ADVANCED_FACE('',(#988,#571,#572,#573,#574,#575),#700,.T.);
#6264=ADVANCED_FACE('',(#989,#576,#577,#578,#579,#580),#701,.F.);
#6265=ADVANCED_FACE('',(#990),#702,.T.);
#6266=ADVANCED_FACE('',(#991),#703,.T.);
#6267=ADVANCED_FACE('',(#992),#704,.T.);
#6268=ADVANCED_FACE('',(#993),#705,.T.);
#6269=ADVANCED_FACE('',(#994),#706,.T.);
#6270=ADVANCED_FACE('',(#995),#707,.F.);
#6271=ADVANCED_FACE('',(#996),#6084,.F.);
#6272=ADVANCED_FACE('',(#997),#708,.F.);
#6273=ADVANCED_FACE('',(#998),#6085,.F.);
#6274=ADVANCED_FACE('',(#999),#709,.F.);
#6275=ADVANCED_FACE('',(#1000),#710,.T.);
#6276=ADVANCED_FACE('',(#1001),#711,.T.);
#6277=ADVANCED_FACE('',(#1002),#712,.T.);
#6278=ADVANCED_FACE('',(#1003),#713,.T.);
#6279=ADVANCED_FACE('',(#1004),#714,.T.);
#6280=ADVANCED_FACE('',(#1005,#581,#582),#715,.F.);
#6281=ADVANCED_FACE('',(#1006),#6086,.F.);
#6282=ADVANCED_FACE('',(#1007),#716,.F.);
#6283=ADVANCED_FACE('',(#1008),#6087,.F.);
#6284=ADVANCED_FACE('',(#1009),#717,.F.);
#6285=ADVANCED_FACE('',(#1010),#718,.T.);
#6286=ADVANCED_FACE('',(#1011),#719,.T.);
#6287=ADVANCED_FACE('',(#1012),#720,.T.);
#6288=ADVANCED_FACE('',(#1013),#721,.T.);
#6289=ADVANCED_FACE('',(#1014),#722,.T.);
#6290=ADVANCED_FACE('',(#1015,#583,#584),#723,.F.);
#6291=ADVANCED_FACE('',(#1016),#6088,.F.);
#6292=ADVANCED_FACE('',(#1017),#724,.T.);
#6293=ADVANCED_FACE('',(#1018,#585),#725,.F.);
#6294=ADVANCED_FACE('',(#1019),#6089,.T.);
#6295=ADVANCED_FACE('',(#1020,#586),#726,.T.);
#6296=ADVANCED_FACE('',(#1021),#6090,.T.);
#6297=ADVANCED_FACE('',(#1022),#727,.F.);
#6298=ADVANCED_FACE('',(#1023),#728,.F.);
#6299=ADVANCED_FACE('',(#1024),#729,.F.);
#6300=ADVANCED_FACE('',(#1025),#730,.F.);
#6301=ADVANCED_FACE('',(#1026),#731,.F.);
#6302=ADVANCED_FACE('',(#1027),#732,.F.);
#6303=ADVANCED_FACE('',(#1028),#733,.F.);
#6304=ADVANCED_FACE('',(#1029),#734,.F.);
#6305=ADVANCED_FACE('',(#1030),#735,.F.);
#6306=ADVANCED_FACE('',(#1031),#736,.F.);
#6307=ADVANCED_FACE('',(#1032),#737,.T.);
#6308=ADVANCED_FACE('',(#1033),#305,.T.);
#6309=ADVANCED_FACE('',(#1034),#6091,.T.);
#6310=ADVANCED_FACE('',(#1035),#306,.T.);
#6311=ADVANCED_FACE('',(#1036,#587),#738,.T.);
#6312=ADVANCED_FACE('',(#1037),#307,.T.);
#6313=ADVANCED_FACE('',(#1038),#6092,.T.);
#6314=ADVANCED_FACE('',(#1039),#303,.F.);
#6315=ADVANCED_FACE('',(#1040),#6093,.T.);
#6316=ADVANCED_FACE('',(#1041),#6094,.F.);
#6317=ADVANCED_FACE('',(#1042),#308,.F.);
#6318=ADVANCED_FACE('',(#1043,#588),#739,.T.);
#6319=ADVANCED_FACE('',(#1044),#6095,.T.);
#6320=ADVANCED_FACE('',(#1045,#589),#740,.T.);
#6321=ADVANCED_FACE('',(#1046),#309,.F.);
#6322=ADVANCED_FACE('',(#1047),#304,.F.);
#6323=ADVANCED_FACE('',(#1048),#6096,.F.);
#6324=ADVANCED_FACE('',(#1049,#590),#741,.T.);
#6325=ADVANCED_FACE('',(#1050),#310,.T.);
#6326=ADVANCED_FACE('',(#1051),#6097,.T.);
#6327=ADVANCED_FACE('',(#1052),#311,.T.);
#6328=ADVANCED_FACE('',(#1053,#591),#742,.T.);
#6329=ADVANCED_FACE('',(#1054),#6098,.F.);
#6330=ADVANCED_FACE('',(#1055),#287,.T.);
#6331=ADVANCED_FACE('',(#1056),#288,.T.);
#6332=ADVANCED_FACE('',(#1057),#289,.T.);
#6333=ADVANCED_FACE('',(#1058),#290,.T.);
#6334=ADVANCED_FACE('',(#1059),#291,.T.);
#6335=ADVANCED_FACE('',(#1060),#292,.T.);
#6336=ADVANCED_FACE('',(#1061),#293,.T.);
#6337=ADVANCED_FACE('',(#1062),#294,.T.);
#6338=ADVANCED_FACE('',(#1063),#295,.F.);
#6339=ADVANCED_FACE('',(#1064),#6099,.T.);
#6340=ADVANCED_FACE('',(#1065),#743,.T.);
#6341=ADVANCED_FACE('',(#1066),#296,.F.);
#6342=ADVANCED_FACE('',(#1067),#744,.T.);
#6343=ADVANCED_FACE('',(#1068),#297,.F.);
#6344=ADVANCED_FACE('',(#1069),#745,.T.);
#6345=ADVANCED_FACE('',(#1070),#298,.F.);
#6346=ADVANCED_FACE('',(#1071),#746,.T.);
#6347=ADVANCED_FACE('',(#1072),#299,.F.);
#6348=ADVANCED_FACE('',(#1073),#747,.T.);
#6349=ADVANCED_FACE('',(#1074),#300,.F.);
#6350=ADVANCED_FACE('',(#1075),#748,.T.);
#6351=ADVANCED_FACE('',(#1076),#301,.F.);
#6352=ADVANCED_FACE('',(#1077),#6100,.F.);
#6353=ADVANCED_FACE('',(#1078),#749,.T.);
#6354=ADVANCED_FACE('',(#1079),#302,.F.);
#6355=ADVANCED_FACE('',(#1080,#592),#750,.T.);
#6356=ADVANCED_FACE('',(#1081),#751,.T.);
#6357=ADVANCED_FACE('',(#1082,#593),#752,.T.);
#6358=ADVANCED_FACE('',(#1083),#6101,.T.);
#6359=ADVANCED_FACE('',(#1084,#594),#753,.T.);
#6360=ADVANCED_FACE('',(#1085),#6102,.F.);
#6361=ADVANCED_FACE('',(#1086,#595),#754,.T.);
#6362=ADVANCED_FACE('',(#1087),#6103,.T.);
#6363=ADVANCED_FACE('',(#1088,#596),#755,.T.);
#6364=ADVANCED_FACE('',(#1089),#6104,.F.);
#6365=ADVANCED_FACE('',(#1090),#756,.F.);
#6366=ADVANCED_FACE('',(#1091),#757,.F.);
#6367=ADVANCED_FACE('',(#1092),#758,.F.);
#6368=ADVANCED_FACE('',(#1093),#759,.F.);
#6369=ADVANCED_FACE('',(#1094),#760,.F.);
#6370=ADVANCED_FACE('',(#1095,#597),#761,.T.);
#6371=ADVANCED_FACE('',(#1096),#6105,.T.);
#6372=ADVANCED_FACE('',(#1097,#598),#762,.T.);
#6373=ADVANCED_FACE('',(#1098),#6106,.T.);
#6374=ADVANCED_FACE('',(#1099,#599),#763,.T.);
#6375=ADVANCED_FACE('',(#1100),#6107,.T.);
#6376=ADVANCED_FACE('',(#1101,#600),#764,.T.);
#6377=ADVANCED_FACE('',(#1102),#6108,.T.);
#6378=ADVANCED_FACE('',(#1103,#601),#765,.T.);
#6379=ADVANCED_FACE('',(#1104),#6109,.T.);
#6380=ADVANCED_FACE('',(#1105,#602),#766,.T.);
#6381=ADVANCED_FACE('',(#1106,#603),#6110,.F.);
#6382=ADVANCED_FACE('',(#1107),#767,.F.);
#6383=ADVANCED_FACE('',(#1108),#768,.F.);
#6384=ADVANCED_FACE('',(#1109),#769,.F.);
#6385=ADVANCED_FACE('',(#1110),#770,.F.);
#6386=ADVANCED_FACE('',(#1111,#604),#771,.T.);
#6387=ADVANCED_FACE('',(#1112,#605),#6111,.T.);
#6388=ADVANCED_FACE('',(#1113,#606),#772,.T.);
#6389=ADVANCED_FACE('',(#1114,#607),#6112,.F.);
#6390=ADVANCED_FACE('',(#1115),#773,.F.);
#6391=ADVANCED_FACE('',(#1116),#774,.F.);
#6392=ADVANCED_FACE('',(#1117),#775,.F.);
#6393=ADVANCED_FACE('',(#1118),#776,.F.);
#6394=ADVANCED_FACE('',(#1119),#777,.F.);
#6395=ADVANCED_FACE('',(#1120),#778,.F.);
#6396=ADVANCED_FACE('',(#1121),#779,.F.);
#6397=ADVANCED_FACE('',(#1122),#780,.F.);
#6398=ADVANCED_FACE('',(#1123,#608),#781,.T.);
#6399=ADVANCED_FACE('',(#1124),#6113,.T.);
#6400=ADVANCED_FACE('',(#1125),#782,.F.);
#6401=ADVANCED_FACE('',(#1126),#783,.T.);
#6402=ADVANCED_FACE('',(#1127),#312,.T.);
#6403=ADVANCED_FACE('',(#1128),#6114,.T.);
#6404=ADVANCED_FACE('',(#1129),#313,.T.);
#6405=ADVANCED_FACE('',(#1130,#609),#784,.T.);
#6406=ADVANCED_FACE('',(#1131),#314,.T.);
#6407=ADVANCED_FACE('',(#1132),#6115,.T.);
#6408=ADVANCED_FACE('',(#1133),#315,.T.);
#6409=ADVANCED_FACE('',(#1134),#6116,.F.);
#6410=ADVANCED_FACE('',(#1135),#6117,.T.);
#6411=ADVANCED_FACE('',(#1136,#610,#611),#785,.F.);
#6412=ADVANCED_FACE('',(#1137),#786,.T.);
#6413=ADVANCED_FACE('',(#1138),#787,.T.);
#6414=ADVANCED_FACE('',(#1139),#788,.T.);
#6415=ADVANCED_FACE('',(#1140),#6118,.T.);
#6416=ADVANCED_FACE('',(#1141),#789,.T.);
#6417=ADVANCED_FACE('',(#1142,#612),#790,.T.);
#6418=ADVANCED_FACE('',(#1143),#791,.T.);
#6419=ADVANCED_FACE('',(#1144,#613),#792,.T.);
#6420=ADVANCED_FACE('',(#1145),#6119,.T.);
#6421=ADVANCED_FACE('',(#1146,#614),#793,.T.);
#6422=ADVANCED_FACE('',(#1147),#6120,.T.);
#6423=ADVANCED_FACE('',(#1148),#6121,.T.);
#6424=ADVANCED_FACE('',(#1149),#6122,.T.);
#6425=ADVANCED_FACE('',(#1150),#794,.T.);
#6426=ADVANCED_FACE('',(#1151),#795,.F.);
#6427=ADVANCED_FACE('',(#1152),#6123,.F.);
#6428=ADVANCED_FACE('',(#1153),#6124,.T.);
#6429=ADVANCED_FACE('',(#1154,#615),#796,.T.);
#6430=ADVANCED_FACE('',(#1155,#616),#797,.F.);
#6431=ADVANCED_FACE('',(#1156),#798,.T.);
#6432=ADVANCED_FACE('',(#1157),#6125,.F.);
#6433=ADVANCED_FACE('',(#1158),#799,.T.);
#6434=ADVANCED_FACE('',(#1159,#617),#6126,.F.);
#6435=ADVANCED_FACE('',(#1160,#618),#6127,.T.);
#6436=ADVANCED_FACE('',(#1161,#619),#800,.T.);
#6437=ADVANCED_FACE('',(#1162,#620),#801,.F.);
#6438=ADVANCED_FACE('',(#1163),#6128,.F.);
#6439=ADVANCED_FACE('',(#1164),#802,.T.);
#6440=ADVANCED_FACE('',(#1165),#6129,.F.);
#6441=ADVANCED_FACE('',(#1166),#803,.F.);
#6442=ADVANCED_FACE('',(#1167,#621),#804,.T.);
#6443=ADVANCED_FACE('',(#1168,#622),#805,.F.);
#6444=ADVANCED_FACE('',(#1169),#6130,.T.);
#6445=ADVANCED_FACE('',(#1170),#6131,.T.);
#6446=ADVANCED_FACE('',(#1171),#6132,.T.);
#6447=ADVANCED_FACE('',(#1172,#623),#806,.T.);
#6448=ADVANCED_FACE('',(#1173,#624),#807,.F.);
#6449=ADVANCED_FACE('',(#1174),#6133,.F.);
#6450=ADVANCED_FACE('',(#1175),#6134,.T.);
#6451=ADVANCED_FACE('',(#1176,#625),#808,.T.);
#6452=ADVANCED_FACE('',(#1177,#626),#809,.F.);
#6453=ADVANCED_FACE('',(#1178),#6135,.F.);
#6454=ADVANCED_FACE('',(#1179),#6136,.T.);
#6455=ADVANCED_FACE('',(#1180,#627),#810,.T.);
#6456=ADVANCED_FACE('',(#1181,#628),#811,.F.);
#6457=ADVANCED_FACE('',(#1182),#6137,.F.);
#6458=ADVANCED_FACE('',(#1183),#6138,.T.);
#6459=ADVANCED_FACE('',(#1184,#629),#812,.T.);
#6460=ADVANCED_FACE('',(#1185,#630),#813,.F.);
#6461=ADVANCED_FACE('',(#1186),#6139,.F.);
#6462=ADVANCED_FACE('',(#1187),#6140,.T.);
#6463=ADVANCED_FACE('',(#1188,#631),#814,.T.);
#6464=ADVANCED_FACE('',(#1189,#632),#815,.F.);
#6465=ADVANCED_FACE('',(#1190),#816,.F.);
#6466=ADVANCED_FACE('',(#1191),#817,.F.);
#6467=ADVANCED_FACE('',(#1192),#818,.F.);
#6468=ADVANCED_FACE('',(#1193),#819,.F.);
#6469=ADVANCED_FACE('',(#1194),#820,.F.);
#6470=ADVANCED_FACE('',(#1195),#821,.F.);
#6471=ADVANCED_FACE('',(#1196),#822,.F.);
#6472=ADVANCED_FACE('',(#1197),#823,.F.);
#6473=ADVANCED_FACE('',(#1198,#633),#824,.T.);
#6474=ADVANCED_FACE('',(#1199),#316,.T.);
#6475=ADVANCED_FACE('',(#1200),#6141,.T.);
#6476=ADVANCED_FACE('',(#1201),#825,.F.);
#6477=ADVANCED_FACE('',(#1202),#826,.F.);
#6478=ADVANCED_FACE('',(#1203),#827,.F.);
#6479=ADVANCED_FACE('',(#1204),#828,.F.);
#6480=ADVANCED_FACE('',(#1205),#829,.F.);
#6481=ADVANCED_FACE('',(#1206),#830,.F.);
#6482=ADVANCED_FACE('',(#1207),#831,.F.);
#6483=ADVANCED_FACE('',(#1208),#832,.F.);
#6484=ADVANCED_FACE('',(#1209),#833,.F.);
#6485=ADVANCED_FACE('',(#1210),#834,.T.);
#6486=ADVANCED_FACE('',(#1211),#317,.T.);
#6487=ADVANCED_FACE('',(#1212),#6142,.T.);
#6488=ADVANCED_FACE('',(#1213),#318,.T.);
#6489=ADVANCED_FACE('',(#1214,#634),#835,.T.);
#6490=ADVANCED_FACE('',(#1215),#319,.T.);
#6491=ADVANCED_FACE('',(#1216),#6143,.T.);
#6492=ADVANCED_FACE('',(#1217),#836,.T.);
#6493=ADVANCED_FACE('',(#1218),#320,.T.);
#6494=ADVANCED_FACE('',(#1219),#6144,.T.);
#6495=ADVANCED_FACE('',(#1220),#321,.T.);
#6496=ADVANCED_FACE('',(#1221,#635),#837,.T.);
#6497=ADVANCED_FACE('',(#1222),#322,.T.);
#6498=ADVANCED_FACE('',(#1223),#6145,.T.);
#6499=ADVANCED_FACE('',(#1224),#323,.T.);
#6500=ADVANCED_FACE('',(#1225),#838,.T.);
#6501=ADVANCED_FACE('',(#1226),#839,.F.);
#6502=ADVANCED_FACE('',(#1227),#840,.F.);
#6503=ADVANCED_FACE('',(#1228),#841,.F.);
#6504=ADVANCED_FACE('',(#1229),#842,.F.);
#6505=ADVANCED_FACE('',(#1230),#843,.F.);
#6506=ADVANCED_FACE('',(#1231),#844,.F.);
#6507=ADVANCED_FACE('',(#1232),#845,.F.);
#6508=ADVANCED_FACE('',(#1233),#846,.F.);
#6509=ADVANCED_FACE('',(#1234),#6146,.F.);
#6510=ADVANCED_FACE('',(#1235),#6147,.F.);
#6511=ADVANCED_FACE('',(#1236),#6148,.T.);
#6512=ADVANCED_FACE('',(#1237),#847,.T.);
#6513=ADVANCED_FACE('',(#1238,#636,#637),#848,.F.);
#6514=ADVANCED_FACE('',(#1239),#849,.T.);
#6515=ADVANCED_FACE('',(#1240),#6149,.T.);
#6516=ADVANCED_FACE('',(#1241,#638,#639),#850,.T.);
#6517=ADVANCED_FACE('',(#1242),#6150,.F.);
#6518=ADVANCED_FACE('',(#1243),#6151,.T.);
#6519=ADVANCED_FACE('',(#1244,#640),#851,.T.);
#6520=ADVANCED_FACE('',(#1245,#641),#852,.F.);
#6521=ADVANCED_FACE('',(#1246),#6152,.F.);
#6522=ADVANCED_FACE('',(#1247),#6153,.T.);
#6523=ADVANCED_FACE('',(#1248,#642),#853,.T.);
#6524=ADVANCED_FACE('',(#1249,#643),#854,.F.);
#6525=ADVANCED_FACE('',(#1250),#6154,.F.);
#6526=ADVANCED_FACE('',(#1251),#855,.F.);
#6527=ADVANCED_FACE('',(#1252,#644),#856,.F.);
#6528=ADVANCED_FACE('',(#1253),#857,.T.);
#6529=ADVANCED_FACE('',(#1254),#858,.F.);
#6530=ADVANCED_FACE('',(#1255),#859,.T.);
#6531=ADVANCED_FACE('',(#1256),#860,.T.);
#6532=ADVANCED_FACE('',(#1257),#861,.T.);
#6533=ADVANCED_FACE('',(#1258),#862,.T.);
#6534=ADVANCED_FACE('',(#1259),#6155,.T.);
#6535=ADVANCED_FACE('',(#1260),#863,.T.);
#6536=ADVANCED_FACE('',(#1261),#6156,.T.);
#6537=ADVANCED_FACE('',(#1262),#864,.F.);
#6538=ADVANCED_FACE('',(#1263),#865,.T.);
#6539=ADVANCED_FACE('',(#1264),#866,.T.);
#6540=ADVANCED_FACE('',(#1265),#6157,.F.);
#6541=ADVANCED_FACE('',(#1266),#867,.T.);
#6542=ADVANCED_FACE('',(#1267,#645),#6158,.F.);
#6543=ADVANCED_FACE('',(#1268,#646),#868,.T.);
#6544=ADVANCED_FACE('',(#1269),#869,.T.);
#6545=ADVANCED_FACE('',(#1270),#870,.T.);
#6546=ADVANCED_FACE('',(#1271),#871,.F.);
#6547=ADVANCED_FACE('',(#1272,#647),#872,.T.);
#6548=ADVANCED_FACE('',(#1273,#648),#873,.T.);
#6549=ADVANCED_FACE('',(#1274,#649),#874,.T.);
#6550=ADVANCED_FACE('',(#1275),#6159,.T.);
#6551=ADVANCED_FACE('',(#1276),#875,.F.);
#6552=ADVANCED_FACE('',(#1277),#6160,.T.);
#6553=ADVANCED_FACE('',(#1278),#876,.T.);
#6554=ADVANCED_FACE('',(#1279),#6161,.T.);
#6555=ADVANCED_FACE('',(#1280),#877,.T.);
#6556=ADVANCED_FACE('',(#1281),#878,.F.);
#6557=ADVANCED_FACE('',(#1282),#879,.F.);
#6558=ADVANCED_FACE('',(#1283),#880,.F.);
#6559=ADVANCED_FACE('',(#1284),#881,.F.);
#6560=ADVANCED_FACE('',(#1285),#882,.F.);
#6561=ADVANCED_FACE('',(#1286),#883,.F.);
#6562=ADVANCED_FACE('',(#1287),#884,.F.);
#6563=ADVANCED_FACE('',(#1288),#885,.F.);
#6564=ADVANCED_FACE('',(#1289,#650),#886,.T.);
#6565=ADVANCED_FACE('',(#1290),#324,.T.);
#6566=ADVANCED_FACE('',(#1291),#6162,.T.);
#6567=ADVANCED_FACE('',(#1292),#325,.T.);
#6568=ADVANCED_FACE('',(#1293),#887,.T.);
#6569=CLOSED_SHELL('',(#6163,#6164,#6165,#6166,#6167,#6168,#6169,#6170,
#6171,#6172,#6173,#6174,#6175,#6176));
#6570=CLOSED_SHELL('',(#6177,#6178,#6179,#6180,#6181,#6182));
#6571=CLOSED_SHELL('',(#6183,#6184,#6185,#6186,#6187,#6188));
#6572=CLOSED_SHELL('',(#6189,#6190,#6191,#6192,#6193,#6194,#6195,#6196,
#6197,#6198,#6199,#6200,#6201,#6202,#6203,#6204,#6205,#6206,#6207,#6208,
#6209,#6210,#6211,#6212,#6213,#6214,#6215,#6216,#6217,#6218,#6219,#6220,
#6221,#6222,#6223,#6224,#6225,#6226));
#6573=CLOSED_SHELL('',(#6227,#6228,#6229,#6230,#6231,#6232,#6233,#6234,
#6235,#6236));
#6574=CLOSED_SHELL('',(#6237,#6238,#6239,#6240,#6241,#6242,#6243,#6244,
#6245,#6246));
#6575=CLOSED_SHELL('',(#6247,#6248,#6249,#6250,#6251,#6252,#6253,#6254,
#6255,#6256,#6257,#6258,#6259,#6260,#6261,#6262,#6263,#6264));
#6576=CLOSED_SHELL('',(#6265,#6266,#6267,#6268,#6269,#6270));
#6577=CLOSED_SHELL('',(#6271,#6272,#6273,#6274,#6275,#6276,#6277,#6278,
#6279,#6280));
#6578=CLOSED_SHELL('',(#6281,#6282,#6283,#6284,#6285,#6286,#6287,#6288,
#6289,#6290));
#6579=CLOSED_SHELL('',(#6291,#6292,#6293,#6294,#6295,#6296,#6297));
#6580=CLOSED_SHELL('',(#6298,#6299,#6300,#6301,#6302,#6303,#6304,#6305));
#6581=CLOSED_SHELL('',(#6306,#6307,#6308,#6309,#6310,#6311,#6312,#6313));
#6582=CLOSED_SHELL('',(#6314,#6315,#6316,#6317,#6318,#6319,#6320,#6321));
#6583=CLOSED_SHELL('',(#6322,#6323,#6324,#6325,#6326,#6327,#6328,#6329));
#6584=CLOSED_SHELL('',(#6330));
#6585=CLOSED_SHELL('',(#6331));
#6586=CLOSED_SHELL('',(#6332));
#6587=CLOSED_SHELL('',(#6333));
#6588=CLOSED_SHELL('',(#6334));
#6589=CLOSED_SHELL('',(#6335));
#6590=CLOSED_SHELL('',(#6336));
#6591=CLOSED_SHELL('',(#6337));
#6592=CLOSED_SHELL('',(#6338,#6339,#6340,#6341,#6342,#6343,#6344,#6345,
#6346,#6347,#6348,#6349,#6350,#6351,#6352,#6353,#6354,#6355,#6356));
#6593=CLOSED_SHELL('',(#6357,#6358,#6359,#6360));
#6594=CLOSED_SHELL('',(#6361,#6362,#6363,#6364));
#6595=CLOSED_SHELL('',(#6365,#6366,#6367,#6368,#6369,#6370,#6371,#6372,
#6373,#6374,#6375,#6376,#6377,#6378,#6379,#6380,#6381));
#6596=CLOSED_SHELL('',(#6382,#6383,#6384,#6385,#6386,#6387,#6388,#6389));
#6597=CLOSED_SHELL('',(#6390,#6391,#6392,#6393,#6394,#6395,#6396,#6397));
#6598=CLOSED_SHELL('',(#6398,#6399,#6400,#6401,#6402,#6403,#6404,#6405,
#6406,#6407,#6408));
#6599=CLOSED_SHELL('',(#6409,#6410,#6411,#6412,#6413,#6414,#6415,#6416,
#6417,#6418,#6419,#6420,#6421,#6422,#6423,#6424,#6425,#6426));
#6600=CLOSED_SHELL('',(#6427,#6428,#6429,#6430));
#6601=CLOSED_SHELL('',(#6431,#6432,#6433,#6434,#6435,#6436,#6437));
#6602=CLOSED_SHELL('',(#6438,#6439,#6440,#6441,#6442,#6443,#6444,#6445,
#6446,#6447,#6448));
#6603=CLOSED_SHELL('',(#6449,#6450,#6451,#6452));
#6604=CLOSED_SHELL('',(#6453,#6454,#6455,#6456));
#6605=CLOSED_SHELL('',(#6457,#6458,#6459,#6460));
#6606=CLOSED_SHELL('',(#6461,#6462,#6463,#6464));
#6607=CLOSED_SHELL('',(#6465,#6466,#6467,#6468,#6469,#6470,#6471,#6472,
#6473,#6474,#6475));
#6608=CLOSED_SHELL('',(#6476,#6477,#6478,#6479,#6480,#6481,#6482,#6483));
#6609=CLOSED_SHELL('',(#6484,#6485,#6486,#6487,#6488,#6489,#6490,#6491));
#6610=CLOSED_SHELL('',(#6492,#6493,#6494,#6495,#6496,#6497,#6498,#6499,
#6500));
#6611=CLOSED_SHELL('',(#6501,#6502,#6503,#6504,#6505,#6506,#6507,#6508));
#6612=CLOSED_SHELL('',(#6509,#6510,#6511,#6512,#6513,#6514,#6515,#6516));
#6613=CLOSED_SHELL('',(#6517,#6518,#6519,#6520));
#6614=CLOSED_SHELL('',(#6521,#6522,#6523,#6524));
#6615=CLOSED_SHELL('',(#6525,#6526,#6527,#6528,#6529,#6530,#6531,#6532,
#6533,#6534,#6535,#6536,#6537,#6538));
#6616=CLOSED_SHELL('',(#6539,#6540,#6541,#6542,#6543,#6544,#6545,#6546,
#6547,#6548));
#6617=CLOSED_SHELL('',(#6549,#6550,#6551,#6552,#6553));
#6618=CLOSED_SHELL('',(#6554,#6555,#6556));
#6619=CLOSED_SHELL('',(#6557,#6558,#6559,#6560,#6561,#6562,#6563,#6564,
#6565,#6566,#6567,#6568));
#6620=DERIVED_UNIT_ELEMENT(#6696,1.);
#6621=DERIVED_UNIT_ELEMENT(#12415,-3.);
#6622=DERIVED_UNIT_ELEMENT(#6696,1.);
#6623=DERIVED_UNIT_ELEMENT(#12415,-3.);
#6624=DERIVED_UNIT_ELEMENT(#6696,1.);
#6625=DERIVED_UNIT_ELEMENT(#12415,-3.);
#6626=DERIVED_UNIT_ELEMENT(#6696,1.);
#6627=DERIVED_UNIT_ELEMENT(#12415,-3.);
#6628=DERIVED_UNIT_ELEMENT(#6696,1.);
#6629=DERIVED_UNIT_ELEMENT(#12415,-3.);
#6630=DERIVED_UNIT_ELEMENT(#6696,1.);
#6631=DERIVED_UNIT_ELEMENT(#12415,-3.);
#6632=DERIVED_UNIT_ELEMENT(#6696,1.);
#6633=DERIVED_UNIT_ELEMENT(#12415,-3.);
#6634=DERIVED_UNIT_ELEMENT(#6696,1.);
#6635=DERIVED_UNIT_ELEMENT(#12415,-3.);
#6636=DERIVED_UNIT_ELEMENT(#6696,1.);
#6637=DERIVED_UNIT_ELEMENT(#12415,-3.);
#6638=DERIVED_UNIT_ELEMENT(#6696,1.);
#6639=DERIVED_UNIT_ELEMENT(#12415,-3.);
#6640=DERIVED_UNIT_ELEMENT(#6696,1.);
#6641=DERIVED_UNIT_ELEMENT(#12415,-3.);
#6642=DERIVED_UNIT_ELEMENT(#6696,1.);
#6643=DERIVED_UNIT_ELEMENT(#12415,-3.);
#6644=DERIVED_UNIT_ELEMENT(#6696,1.);
#6645=DERIVED_UNIT_ELEMENT(#12415,-3.);
#6646=DERIVED_UNIT_ELEMENT(#6696,1.);
#6647=DERIVED_UNIT_ELEMENT(#12415,-3.);
#6648=DERIVED_UNIT_ELEMENT(#6696,1.);
#6649=DERIVED_UNIT_ELEMENT(#12415,-3.);
#6650=DERIVED_UNIT_ELEMENT(#6696,1.);
#6651=DERIVED_UNIT_ELEMENT(#12415,-3.);
#6652=DERIVED_UNIT_ELEMENT(#6696,1.);
#6653=DERIVED_UNIT_ELEMENT(#12415,-3.);
#6654=DERIVED_UNIT_ELEMENT(#6696,1.);
#6655=DERIVED_UNIT_ELEMENT(#12415,-3.);
#6656=DERIVED_UNIT_ELEMENT(#6696,1.);
#6657=DERIVED_UNIT_ELEMENT(#12415,-3.);
#6658=DERIVED_UNIT_ELEMENT(#6696,1.);
#6659=DERIVED_UNIT_ELEMENT(#12415,-3.);
#6660=DERIVED_UNIT_ELEMENT(#6696,1.);
#6661=DERIVED_UNIT_ELEMENT(#12415,-3.);
#6662=DERIVED_UNIT_ELEMENT(#6696,1.);
#6663=DERIVED_UNIT_ELEMENT(#12415,-3.);
#6664=DERIVED_UNIT_ELEMENT(#6696,1.);
#6665=DERIVED_UNIT_ELEMENT(#12415,-3.);
#6666=DERIVED_UNIT_ELEMENT(#6696,1.);
#6667=DERIVED_UNIT_ELEMENT(#12415,-3.);
#6668=DERIVED_UNIT_ELEMENT(#6696,1.);
#6669=DERIVED_UNIT_ELEMENT(#12415,-3.);
#6670=DERIVED_UNIT_ELEMENT(#6696,1.);
#6671=DERIVED_UNIT_ELEMENT(#12415,-3.);
#6672=DERIVED_UNIT_ELEMENT(#6696,1.);
#6673=DERIVED_UNIT_ELEMENT(#12415,-3.);
#6674=DERIVED_UNIT_ELEMENT(#6696,1.);
#6675=DERIVED_UNIT_ELEMENT(#12415,-3.);
#6676=DERIVED_UNIT_ELEMENT(#6696,1.);
#6677=DERIVED_UNIT_ELEMENT(#12415,-3.);
#6678=DERIVED_UNIT_ELEMENT(#6696,1.);
#6679=DERIVED_UNIT_ELEMENT(#12415,-3.);
#6680=DERIVED_UNIT_ELEMENT(#6696,1.);
#6681=DERIVED_UNIT_ELEMENT(#12415,-3.);
#6682=DERIVED_UNIT_ELEMENT(#6696,1.);
#6683=DERIVED_UNIT_ELEMENT(#12415,-3.);
#6684=DERIVED_UNIT_ELEMENT(#6696,1.);
#6685=DERIVED_UNIT_ELEMENT(#12415,-3.);
#6686=DERIVED_UNIT_ELEMENT(#6696,1.);
#6687=DERIVED_UNIT_ELEMENT(#12415,-3.);
#6688=DERIVED_UNIT_ELEMENT(#6696,1.);
#6689=DERIVED_UNIT_ELEMENT(#12415,-3.);
#6690=DERIVED_UNIT_ELEMENT(#6696,1.);
#6691=DERIVED_UNIT_ELEMENT(#12415,-3.);
#6692=DERIVED_UNIT_ELEMENT(#6696,1.);
#6693=DERIVED_UNIT_ELEMENT(#12415,-3.);
#6694=DERIVED_UNIT_ELEMENT(#6696,1.);
#6695=DERIVED_UNIT_ELEMENT(#12415,-3.);
#6696=(
MASS_UNIT()
NAMED_UNIT(*)
SI_UNIT(.KILO.,.GRAM.)
);
#6697=DERIVED_UNIT((#6620,#6621));
#6698=DERIVED_UNIT((#6622,#6623));
#6699=DERIVED_UNIT((#6624,#6625));
#6700=DERIVED_UNIT((#6626,#6627));
#6701=DERIVED_UNIT((#6628,#6629));
#6702=DERIVED_UNIT((#6630,#6631));
#6703=DERIVED_UNIT((#6632,#6633));
#6704=DERIVED_UNIT((#6634,#6635));
#6705=DERIVED_UNIT((#6636,#6637));
#6706=DERIVED_UNIT((#6638,#6639));
#6707=DERIVED_UNIT((#6640,#6641));
#6708=DERIVED_UNIT((#6642,#6643));
#6709=DERIVED_UNIT((#6644,#6645));
#6710=DERIVED_UNIT((#6646,#6647));
#6711=DERIVED_UNIT((#6648,#6649));
#6712=DERIVED_UNIT((#6650,#6651));
#6713=DERIVED_UNIT((#6652,#6653));
#6714=DERIVED_UNIT((#6654,#6655));
#6715=DERIVED_UNIT((#6656,#6657));
#6716=DERIVED_UNIT((#6658,#6659));
#6717=DERIVED_UNIT((#6660,#6661));
#6718=DERIVED_UNIT((#6662,#6663));
#6719=DERIVED_UNIT((#6664,#6665));
#6720=DERIVED_UNIT((#6666,#6667));
#6721=DERIVED_UNIT((#6668,#6669));
#6722=DERIVED_UNIT((#6670,#6671));
#6723=DERIVED_UNIT((#6672,#6673));
#6724=DERIVED_UNIT((#6674,#6675));
#6725=DERIVED_UNIT((#6676,#6677));
#6726=DERIVED_UNIT((#6678,#6679));
#6727=DERIVED_UNIT((#6680,#6681));
#6728=DERIVED_UNIT((#6682,#6683));
#6729=DERIVED_UNIT((#6684,#6685));
#6730=DERIVED_UNIT((#6686,#6687));
#6731=DERIVED_UNIT((#6688,#6689));
#6732=DERIVED_UNIT((#6690,#6691));
#6733=DERIVED_UNIT((#6692,#6693));
#6734=DERIVED_UNIT((#6694,#6695));
#6735=MEASURE_REPRESENTATION_ITEM('density measure',
POSITIVE_RATIO_MEASURE(7850.),#6697);
#6736=MEASURE_REPRESENTATION_ITEM('density measure',
POSITIVE_RATIO_MEASURE(7850.),#6698);
#6737=MEASURE_REPRESENTATION_ITEM('density measure',
POSITIVE_RATIO_MEASURE(7850.),#6699);
#6738=MEASURE_REPRESENTATION_ITEM('density measure',
POSITIVE_RATIO_MEASURE(7850.),#6700);
#6739=MEASURE_REPRESENTATION_ITEM('density measure',
POSITIVE_RATIO_MEASURE(7850.),#6701);
#6740=MEASURE_REPRESENTATION_ITEM('density measure',
POSITIVE_RATIO_MEASURE(7850.),#6702);
#6741=MEASURE_REPRESENTATION_ITEM('density measure',
POSITIVE_RATIO_MEASURE(7850.),#6703);
#6742=MEASURE_REPRESENTATION_ITEM('density measure',
POSITIVE_RATIO_MEASURE(7850.),#6704);
#6743=MEASURE_REPRESENTATION_ITEM('density measure',
POSITIVE_RATIO_MEASURE(7850.),#6705);
#6744=MEASURE_REPRESENTATION_ITEM('density measure',
POSITIVE_RATIO_MEASURE(7850.),#6706);
#6745=MEASURE_REPRESENTATION_ITEM('density measure',
POSITIVE_RATIO_MEASURE(7850.),#6707);
#6746=MEASURE_REPRESENTATION_ITEM('density measure',
POSITIVE_RATIO_MEASURE(7850.),#6708);
#6747=MEASURE_REPRESENTATION_ITEM('density measure',
POSITIVE_RATIO_MEASURE(7850.),#6709);
#6748=MEASURE_REPRESENTATION_ITEM('density measure',
POSITIVE_RATIO_MEASURE(7850.),#6710);
#6749=MEASURE_REPRESENTATION_ITEM('density measure',
POSITIVE_RATIO_MEASURE(7850.),#6711);
#6750=MEASURE_REPRESENTATION_ITEM('density measure',
POSITIVE_RATIO_MEASURE(7850.),#6712);
#6751=MEASURE_REPRESENTATION_ITEM('density measure',
POSITIVE_RATIO_MEASURE(7850.),#6713);
#6752=MEASURE_REPRESENTATION_ITEM('density measure',
POSITIVE_RATIO_MEASURE(7850.),#6714);
#6753=MEASURE_REPRESENTATION_ITEM('density measure',
POSITIVE_RATIO_MEASURE(7850.),#6715);
#6754=MEASURE_REPRESENTATION_ITEM('density measure',
POSITIVE_RATIO_MEASURE(7850.),#6716);
#6755=MEASURE_REPRESENTATION_ITEM('density measure',
POSITIVE_RATIO_MEASURE(7850.),#6717);
#6756=MEASURE_REPRESENTATION_ITEM('density measure',
POSITIVE_RATIO_MEASURE(7850.),#6718);
#6757=MEASURE_REPRESENTATION_ITEM('density measure',
POSITIVE_RATIO_MEASURE(7850.),#6719);
#6758=MEASURE_REPRESENTATION_ITEM('density measure',
POSITIVE_RATIO_MEASURE(7850.),#6720);
#6759=MEASURE_REPRESENTATION_ITEM('density measure',
POSITIVE_RATIO_MEASURE(7850.),#6721);
#6760=MEASURE_REPRESENTATION_ITEM('density measure',
POSITIVE_RATIO_MEASURE(7850.),#6722);
#6761=MEASURE_REPRESENTATION_ITEM('density measure',
POSITIVE_RATIO_MEASURE(7850.),#6723);
#6762=MEASURE_REPRESENTATION_ITEM('density measure',
POSITIVE_RATIO_MEASURE(7850.),#6724);
#6763=MEASURE_REPRESENTATION_ITEM('density measure',
POSITIVE_RATIO_MEASURE(7850.),#6725);
#6764=MEASURE_REPRESENTATION_ITEM('density measure',
POSITIVE_RATIO_MEASURE(7850.),#6726);
#6765=MEASURE_REPRESENTATION_ITEM('density measure',
POSITIVE_RATIO_MEASURE(7850.),#6727);
#6766=MEASURE_REPRESENTATION_ITEM('density measure',
POSITIVE_RATIO_MEASURE(7850.),#6728);
#6767=MEASURE_REPRESENTATION_ITEM('density measure',
POSITIVE_RATIO_MEASURE(7850.),#6729);
#6768=MEASURE_REPRESENTATION_ITEM('density measure',
POSITIVE_RATIO_MEASURE(7850.),#6730);
#6769=MEASURE_REPRESENTATION_ITEM('density measure',
POSITIVE_RATIO_MEASURE(7850.),#6731);
#6770=MEASURE_REPRESENTATION_ITEM('density measure',
POSITIVE_RATIO_MEASURE(7850.),#6732);
#6771=MEASURE_REPRESENTATION_ITEM('density measure',
POSITIVE_RATIO_MEASURE(7850.),#6733);
#6772=MEASURE_REPRESENTATION_ITEM('density measure',
POSITIVE_RATIO_MEASURE(7850.),#6734);
#6773=PROPERTY_DEFINITION_REPRESENTATION(#6963,#6849);
#6774=PROPERTY_DEFINITION_REPRESENTATION(#6964,#6850);
#6775=PROPERTY_DEFINITION_REPRESENTATION(#6965,#6851);
#6776=PROPERTY_DEFINITION_REPRESENTATION(#6966,#6852);
#6777=PROPERTY_DEFINITION_REPRESENTATION(#6967,#6853);
#6778=PROPERTY_DEFINITION_REPRESENTATION(#6968,#6854);
#6779=PROPERTY_DEFINITION_REPRESENTATION(#6969,#6855);
#6780=PROPERTY_DEFINITION_REPRESENTATION(#6970,#6856);
#6781=PROPERTY_DEFINITION_REPRESENTATION(#6971,#6857);
#6782=PROPERTY_DEFINITION_REPRESENTATION(#6972,#6858);
#6783=PROPERTY_DEFINITION_REPRESENTATION(#6973,#6859);
#6784=PROPERTY_DEFINITION_REPRESENTATION(#6974,#6860);
#6785=PROPERTY_DEFINITION_REPRESENTATION(#6975,#6861);
#6786=PROPERTY_DEFINITION_REPRESENTATION(#6976,#6862);
#6787=PROPERTY_DEFINITION_REPRESENTATION(#6977,#6863);
#6788=PROPERTY_DEFINITION_REPRESENTATION(#6978,#6864);
#6789=PROPERTY_DEFINITION_REPRESENTATION(#6979,#6865);
#6790=PROPERTY_DEFINITION_REPRESENTATION(#6980,#6866);
#6791=PROPERTY_DEFINITION_REPRESENTATION(#6981,#6867);
#6792=PROPERTY_DEFINITION_REPRESENTATION(#6982,#6868);
#6793=PROPERTY_DEFINITION_REPRESENTATION(#6983,#6869);
#6794=PROPERTY_DEFINITION_REPRESENTATION(#6984,#6870);
#6795=PROPERTY_DEFINITION_REPRESENTATION(#6985,#6871);
#6796=PROPERTY_DEFINITION_REPRESENTATION(#6986,#6872);
#6797=PROPERTY_DEFINITION_REPRESENTATION(#6987,#6873);
#6798=PROPERTY_DEFINITION_REPRESENTATION(#6988,#6874);
#6799=PROPERTY_DEFINITION_REPRESENTATION(#6989,#6875);
#6800=PROPERTY_DEFINITION_REPRESENTATION(#6990,#6876);
#6801=PROPERTY_DEFINITION_REPRESENTATION(#6991,#6877);
#6802=PROPERTY_DEFINITION_REPRESENTATION(#6992,#6878);
#6803=PROPERTY_DEFINITION_REPRESENTATION(#6993,#6879);
#6804=PROPERTY_DEFINITION_REPRESENTATION(#6994,#6880);
#6805=PROPERTY_DEFINITION_REPRESENTATION(#6995,#6881);
#6806=PROPERTY_DEFINITION_REPRESENTATION(#6996,#6882);
#6807=PROPERTY_DEFINITION_REPRESENTATION(#6997,#6883);
#6808=PROPERTY_DEFINITION_REPRESENTATION(#6998,#6884);
#6809=PROPERTY_DEFINITION_REPRESENTATION(#6999,#6885);
#6810=PROPERTY_DEFINITION_REPRESENTATION(#7000,#6886);
#6811=PROPERTY_DEFINITION_REPRESENTATION(#7001,#6887);
#6812=PROPERTY_DEFINITION_REPRESENTATION(#7002,#6888);
#6813=PROPERTY_DEFINITION_REPRESENTATION(#7003,#6889);
#6814=PROPERTY_DEFINITION_REPRESENTATION(#7004,#6890);
#6815=PROPERTY_DEFINITION_REPRESENTATION(#7005,#6891);
#6816=PROPERTY_DEFINITION_REPRESENTATION(#7006,#6892);
#6817=PROPERTY_DEFINITION_REPRESENTATION(#7007,#6893);
#6818=PROPERTY_DEFINITION_REPRESENTATION(#7008,#6894);
#6819=PROPERTY_DEFINITION_REPRESENTATION(#7009,#6895);
#6820=PROPERTY_DEFINITION_REPRESENTATION(#7010,#6896);
#6821=PROPERTY_DEFINITION_REPRESENTATION(#7011,#6897);
#6822=PROPERTY_DEFINITION_REPRESENTATION(#7012,#6898);
#6823=PROPERTY_DEFINITION_REPRESENTATION(#7013,#6899);
#6824=PROPERTY_DEFINITION_REPRESENTATION(#7014,#6900);
#6825=PROPERTY_DEFINITION_REPRESENTATION(#7015,#6901);
#6826=PROPERTY_DEFINITION_REPRESENTATION(#7016,#6902);
#6827=PROPERTY_DEFINITION_REPRESENTATION(#7017,#6903);
#6828=PROPERTY_DEFINITION_REPRESENTATION(#7018,#6904);
#6829=PROPERTY_DEFINITION_REPRESENTATION(#7019,#6905);
#6830=PROPERTY_DEFINITION_REPRESENTATION(#7020,#6906);
#6831=PROPERTY_DEFINITION_REPRESENTATION(#7021,#6907);
#6832=PROPERTY_DEFINITION_REPRESENTATION(#7022,#6908);
#6833=PROPERTY_DEFINITION_REPRESENTATION(#7023,#6909);
#6834=PROPERTY_DEFINITION_REPRESENTATION(#7024,#6910);
#6835=PROPERTY_DEFINITION_REPRESENTATION(#7025,#6911);
#6836=PROPERTY_DEFINITION_REPRESENTATION(#7026,#6912);
#6837=PROPERTY_DEFINITION_REPRESENTATION(#7027,#6913);
#6838=PROPERTY_DEFINITION_REPRESENTATION(#7028,#6914);
#6839=PROPERTY_DEFINITION_REPRESENTATION(#7029,#6915);
#6840=PROPERTY_DEFINITION_REPRESENTATION(#7030,#6916);
#6841=PROPERTY_DEFINITION_REPRESENTATION(#7031,#6917);
#6842=PROPERTY_DEFINITION_REPRESENTATION(#7032,#6918);
#6843=PROPERTY_DEFINITION_REPRESENTATION(#7033,#6919);
#6844=PROPERTY_DEFINITION_REPRESENTATION(#7034,#6920);
#6845=PROPERTY_DEFINITION_REPRESENTATION(#7035,#6921);
#6846=PROPERTY_DEFINITION_REPRESENTATION(#7036,#6922);
#6847=PROPERTY_DEFINITION_REPRESENTATION(#7037,#6923);
#6848=PROPERTY_DEFINITION_REPRESENTATION(#7038,#6924);
#6849=REPRESENTATION('material name',(#6925),#12370);
#6850=REPRESENTATION('density',(#6735),#12370);
#6851=REPRESENTATION('material name',(#6926),#12371);
#6852=REPRESENTATION('density',(#6736),#12371);
#6853=REPRESENTATION('material name',(#6927),#12372);
#6854=REPRESENTATION('density',(#6737),#12372);
#6855=REPRESENTATION('material name',(#6928),#12373);
#6856=REPRESENTATION('density',(#6738),#12373);
#6857=REPRESENTATION('material name',(#6929),#12374);
#6858=REPRESENTATION('density',(#6739),#12374);
#6859=REPRESENTATION('material name',(#6930),#12375);
#6860=REPRESENTATION('density',(#6740),#12375);
#6861=REPRESENTATION('material name',(#6931),#12376);
#6862=REPRESENTATION('density',(#6741),#12376);
#6863=REPRESENTATION('material name',(#6932),#12377);
#6864=REPRESENTATION('density',(#6742),#12377);
#6865=REPRESENTATION('material name',(#6933),#12378);
#6866=REPRESENTATION('density',(#6743),#12378);
#6867=REPRESENTATION('material name',(#6934),#12379);
#6868=REPRESENTATION('density',(#6744),#12379);
#6869=REPRESENTATION('material name',(#6935),#12380);
#6870=REPRESENTATION('density',(#6745),#12380);
#6871=REPRESENTATION('material name',(#6936),#12381);
#6872=REPRESENTATION('density',(#6746),#12381);
#6873=REPRESENTATION('material name',(#6937),#12383);
#6874=REPRESENTATION('density',(#6747),#12383);
#6875=REPRESENTATION('material name',(#6938),#12384);
#6876=REPRESENTATION('density',(#6748),#12384);
#6877=REPRESENTATION('material name',(#6939),#12385);
#6878=REPRESENTATION('density',(#6749),#12385);
#6879=REPRESENTATION('material name',(#6940),#12386);
#6880=REPRESENTATION('density',(#6750),#12386);
#6881=REPRESENTATION('material name',(#6941),#12387);
#6882=REPRESENTATION('density',(#6751),#12387);
#6883=REPRESENTATION('material name',(#6942),#12389);
#6884=REPRESENTATION('density',(#6752),#12389);
#6885=REPRESENTATION('material name',(#6943),#12390);
#6886=REPRESENTATION('density',(#6753),#12390);
#6887=REPRESENTATION('material name',(#6944),#12391);
#6888=REPRESENTATION('density',(#6754),#12391);
#6889=REPRESENTATION('material name',(#6945),#12393);
#6890=REPRESENTATION('density',(#6755),#12393);
#6891=REPRESENTATION('material name',(#6946),#12394);
#6892=REPRESENTATION('density',(#6756),#12394);
#6893=REPRESENTATION('material name',(#6947),#12395);
#6894=REPRESENTATION('density',(#6757),#12395);
#6895=REPRESENTATION('material name',(#6948),#12396);
#6896=REPRESENTATION('density',(#6758),#12396);
#6897=REPRESENTATION('material name',(#6949),#12397);
#6898=REPRESENTATION('density',(#6759),#12397);
#6899=REPRESENTATION('material name',(#6950),#12398);
#6900=REPRESENTATION('density',(#6760),#12398);
#6901=REPRESENTATION('material name',(#6951),#12399);
#6902=REPRESENTATION('density',(#6761),#12399);
#6903=REPRESENTATION('material name',(#6952),#12400);
#6904=REPRESENTATION('density',(#6762),#12400);
#6905=REPRESENTATION('material name',(#6953),#12401);
#6906=REPRESENTATION('density',(#6763),#12401);
#6907=REPRESENTATION('material name',(#6954),#12402);
#6908=REPRESENTATION('density',(#6764),#12402);
#6909=REPRESENTATION('material name',(#6955),#12403);
#6910=REPRESENTATION('density',(#6765),#12403);
#6911=REPRESENTATION('material name',(#6956),#12405);
#6912=REPRESENTATION('density',(#6766),#12405);
#6913=REPRESENTATION('material name',(#6957),#12406);
#6914=REPRESENTATION('density',(#6767),#12406);
#6915=REPRESENTATION('material name',(#6958),#12407);
#6916=REPRESENTATION('density',(#6768),#12407);
#6917=REPRESENTATION('material name',(#6959),#12409);
#6918=REPRESENTATION('density',(#6769),#12409);
#6919=REPRESENTATION('material name',(#6960),#12410);
#6920=REPRESENTATION('density',(#6770),#12410);
#6921=REPRESENTATION('material name',(#6961),#12411);
#6922=REPRESENTATION('density',(#6771),#12411);
#6923=REPRESENTATION('material name',(#6962),#12412);
#6924=REPRESENTATION('density',(#6772),#12412);
#6925=DESCRIPTIVE_REPRESENTATION_ITEM('Steel','Steel');
#6926=DESCRIPTIVE_REPRESENTATION_ITEM('Steel','Steel');
#6927=DESCRIPTIVE_REPRESENTATION_ITEM('Steel','Steel');
#6928=DESCRIPTIVE_REPRESENTATION_ITEM('Steel','Steel');
#6929=DESCRIPTIVE_REPRESENTATION_ITEM('Steel','Steel');
#6930=DESCRIPTIVE_REPRESENTATION_ITEM('Steel','Steel');
#6931=DESCRIPTIVE_REPRESENTATION_ITEM('Steel','Steel');
#6932=DESCRIPTIVE_REPRESENTATION_ITEM('Steel','Steel');
#6933=DESCRIPTIVE_REPRESENTATION_ITEM('Steel','Steel');
#6934=DESCRIPTIVE_REPRESENTATION_ITEM('Steel','Steel');
#6935=DESCRIPTIVE_REPRESENTATION_ITEM('Steel','Steel');
#6936=DESCRIPTIVE_REPRESENTATION_ITEM('Steel','Steel');
#6937=DESCRIPTIVE_REPRESENTATION_ITEM('Steel','Steel');
#6938=DESCRIPTIVE_REPRESENTATION_ITEM('Steel','Steel');
#6939=DESCRIPTIVE_REPRESENTATION_ITEM('Steel','Steel');
#6940=DESCRIPTIVE_REPRESENTATION_ITEM('Steel','Steel');
#6941=DESCRIPTIVE_REPRESENTATION_ITEM('Steel','Steel');
#6942=DESCRIPTIVE_REPRESENTATION_ITEM('Steel','Steel');
#6943=DESCRIPTIVE_REPRESENTATION_ITEM('Steel','Steel');
#6944=DESCRIPTIVE_REPRESENTATION_ITEM('Steel','Steel');
#6945=DESCRIPTIVE_REPRESENTATION_ITEM('Steel','Steel');
#6946=DESCRIPTIVE_REPRESENTATION_ITEM('Steel','Steel');
#6947=DESCRIPTIVE_REPRESENTATION_ITEM('Steel','Steel');
#6948=DESCRIPTIVE_REPRESENTATION_ITEM('Steel','Steel');
#6949=DESCRIPTIVE_REPRESENTATION_ITEM('Steel','Steel');
#6950=DESCRIPTIVE_REPRESENTATION_ITEM('Steel','Steel');
#6951=DESCRIPTIVE_REPRESENTATION_ITEM('Steel','Steel');
#6952=DESCRIPTIVE_REPRESENTATION_ITEM('Steel','Steel');
#6953=DESCRIPTIVE_REPRESENTATION_ITEM('Steel','Steel');
#6954=DESCRIPTIVE_REPRESENTATION_ITEM('Steel','Steel');
#6955=DESCRIPTIVE_REPRESENTATION_ITEM('Steel','Steel');
#6956=DESCRIPTIVE_REPRESENTATION_ITEM('Steel','Steel');
#6957=DESCRIPTIVE_REPRESENTATION_ITEM('Steel','Steel');
#6958=DESCRIPTIVE_REPRESENTATION_ITEM('Steel','Steel');
#6959=DESCRIPTIVE_REPRESENTATION_ITEM('Steel','Steel');
#6960=DESCRIPTIVE_REPRESENTATION_ITEM('Steel','Steel');
#6961=DESCRIPTIVE_REPRESENTATION_ITEM('Steel','Steel');
#6962=DESCRIPTIVE_REPRESENTATION_ITEM('Steel','Steel');
#6963=PROPERTY_DEFINITION('material property','material name',#12619);
#6964=PROPERTY_DEFINITION('material property','density of part',#12619);
#6965=PROPERTY_DEFINITION('material property','material name',#12620);
#6966=PROPERTY_DEFINITION('material property','density of part',#12620);
#6967=PROPERTY_DEFINITION('material property','material name',#12621);
#6968=PROPERTY_DEFINITION('material property','density of part',#12621);
#6969=PROPERTY_DEFINITION('material property','material name',#12622);
#6970=PROPERTY_DEFINITION('material property','density of part',#12622);
#6971=PROPERTY_DEFINITION('material property','material name',#12623);
#6972=PROPERTY_DEFINITION('material property','density of part',#12623);
#6973=PROPERTY_DEFINITION('material property','material name',#12624);
#6974=PROPERTY_DEFINITION('material property','density of part',#12624);
#6975=PROPERTY_DEFINITION('material property','material name',#12625);
#6976=PROPERTY_DEFINITION('material property','density of part',#12625);
#6977=PROPERTY_DEFINITION('material property','material name',#12626);
#6978=PROPERTY_DEFINITION('material property','density of part',#12626);
#6979=PROPERTY_DEFINITION('material property','material name',#12627);
#6980=PROPERTY_DEFINITION('material property','density of part',#12627);
#6981=PROPERTY_DEFINITION('material property','material name',#12628);
#6982=PROPERTY_DEFINITION('material property','density of part',#12628);
#6983=PROPERTY_DEFINITION('material property','material name',#12629);
#6984=PROPERTY_DEFINITION('material property','density of part',#12629);
#6985=PROPERTY_DEFINITION('material property','material name',#12630);
#6986=PROPERTY_DEFINITION('material property','density of part',#12630);
#6987=PROPERTY_DEFINITION('material property','material name',#12632);
#6988=PROPERTY_DEFINITION('material property','density of part',#12632);
#6989=PROPERTY_DEFINITION('material property','material name',#12633);
#6990=PROPERTY_DEFINITION('material property','density of part',#12633);
#6991=PROPERTY_DEFINITION('material property','material name',#12634);
#6992=PROPERTY_DEFINITION('material property','density of part',#12634);
#6993=PROPERTY_DEFINITION('material property','material name',#12635);
#6994=PROPERTY_DEFINITION('material property','density of part',#12635);
#6995=PROPERTY_DEFINITION('material property','material name',#12636);
#6996=PROPERTY_DEFINITION('material property','density of part',#12636);
#6997=PROPERTY_DEFINITION('material property','material name',#12638);
#6998=PROPERTY_DEFINITION('material property','density of part',#12638);
#6999=PROPERTY_DEFINITION('material property','material name',#12639);
#7000=PROPERTY_DEFINITION('material property','density of part',#12639);
#7001=PROPERTY_DEFINITION('material property','material name',#12640);
#7002=PROPERTY_DEFINITION('material property','density of part',#12640);
#7003=PROPERTY_DEFINITION('material property','material name',#12642);
#7004=PROPERTY_DEFINITION('material property','density of part',#12642);
#7005=PROPERTY_DEFINITION('material property','material name',#12643);
#7006=PROPERTY_DEFINITION('material property','density of part',#12643);
#7007=PROPERTY_DEFINITION('material property','material name',#12644);
#7008=PROPERTY_DEFINITION('material property','density of part',#12644);
#7009=PROPERTY_DEFINITION('material property','material name',#12645);
#7010=PROPERTY_DEFINITION('material property','density of part',#12645);
#7011=PROPERTY_DEFINITION('material property','material name',#12646);
#7012=PROPERTY_DEFINITION('material property','density of part',#12646);
#7013=PROPERTY_DEFINITION('material property','material name',#12647);
#7014=PROPERTY_DEFINITION('material property','density of part',#12647);
#7015=PROPERTY_DEFINITION('material property','material name',#12648);
#7016=PROPERTY_DEFINITION('material property','density of part',#12648);
#7017=PROPERTY_DEFINITION('material property','material name',#12649);
#7018=PROPERTY_DEFINITION('material property','density of part',#12649);
#7019=PROPERTY_DEFINITION('material property','material name',#12650);
#7020=PROPERTY_DEFINITION('material property','density of part',#12650);
#7021=PROPERTY_DEFINITION('material property','material name',#12651);
#7022=PROPERTY_DEFINITION('material property','density of part',#12651);
#7023=PROPERTY_DEFINITION('material property','material name',#12652);
#7024=PROPERTY_DEFINITION('material property','density of part',#12652);
#7025=PROPERTY_DEFINITION('material property','material name',#12654);
#7026=PROPERTY_DEFINITION('material property','density of part',#12654);
#7027=PROPERTY_DEFINITION('material property','material name',#12655);
#7028=PROPERTY_DEFINITION('material property','density of part',#12655);
#7029=PROPERTY_DEFINITION('material property','material name',#12656);
#7030=PROPERTY_DEFINITION('material property','density of part',#12656);
#7031=PROPERTY_DEFINITION('material property','material name',#12658);
#7032=PROPERTY_DEFINITION('material property','density of part',#12658);
#7033=PROPERTY_DEFINITION('material property','material name',#12659);
#7034=PROPERTY_DEFINITION('material property','density of part',#12659);
#7035=PROPERTY_DEFINITION('material property','material name',#12660);
#7036=PROPERTY_DEFINITION('material property','density of part',#12660);
#7037=PROPERTY_DEFINITION('material property','material name',#12661);
#7038=PROPERTY_DEFINITION('material property','density of part',#12661);
#7039=AXIS2_PLACEMENT_3D('',#10045,#7894,#7895);
#7040=AXIS2_PLACEMENT_3D('',#10046,#7896,#7897);
#7041=AXIS2_PLACEMENT_3D('',#10047,#7898,#7899);
#7042=AXIS2_PLACEMENT_3D('',#10048,#7900,#7901);
#7043=AXIS2_PLACEMENT_3D('',#10050,#7902,#7903);
#7044=AXIS2_PLACEMENT_3D('',#10053,#7905,#7906);
#7045=AXIS2_PLACEMENT_3D('',#10054,#7907,#7908);
#7046=AXIS2_PLACEMENT_3D('',#10056,#7909,#7910);
#7047=AXIS2_PLACEMENT_3D('',#10059,#7912,#7913);
#7048=AXIS2_PLACEMENT_3D('',#10060,#7914,#7915);
#7049=AXIS2_PLACEMENT_3D('',#10062,#7916,#7917);
#7050=AXIS2_PLACEMENT_3D('',#10065,#7919,#7920);
#7051=AXIS2_PLACEMENT_3D('',#10066,#7921,#7922);
#7052=AXIS2_PLACEMENT_3D('',#10068,#7923,#7924);
#7053=AXIS2_PLACEMENT_3D('',#10071,#7926,#7927);
#7054=AXIS2_PLACEMENT_3D('',#10072,#7928,#7929);
#7055=AXIS2_PLACEMENT_3D('',#10074,#7930,#7931);
#7056=AXIS2_PLACEMENT_3D('',#10077,#7933,#7934);
#7057=AXIS2_PLACEMENT_3D('',#10078,#7935,#7936);
#7058=AXIS2_PLACEMENT_3D('',#10080,#7937,#7938);
#7059=AXIS2_PLACEMENT_3D('',#10083,#7940,#7941);
#7060=AXIS2_PLACEMENT_3D('',#10084,#7942,#7943);
#7061=AXIS2_PLACEMENT_3D('',#10086,#7944,#7945);
#7062=AXIS2_PLACEMENT_3D('',#10089,#7947,#7948);
#7063=AXIS2_PLACEMENT_3D('',#10090,#7949,#7950);
#7064=AXIS2_PLACEMENT_3D('',#10092,#7951,#7952);
#7065=AXIS2_PLACEMENT_3D('',#10095,#7954,#7955);
#7066=AXIS2_PLACEMENT_3D('',#10096,#7956,#7957);
#7067=AXIS2_PLACEMENT_3D('',#10105,#7962,#7963);
#7068=AXIS2_PLACEMENT_3D('',#10111,#7967,#7968);
#7069=AXIS2_PLACEMENT_3D('',#10117,#7972,#7973);
#7070=AXIS2_PLACEMENT_3D('',#10120,#7976,#7977);
#7071=AXIS2_PLACEMENT_3D('',#10121,#7978,#7979);
#7072=AXIS2_PLACEMENT_3D('',#10122,#7980,#7981);
#7073=AXIS2_PLACEMENT_3D('',#10123,#7982,#7983);
#7074=AXIS2_PLACEMENT_3D('',#10132,#7988,#7989);
#7075=AXIS2_PLACEMENT_3D('',#10138,#7993,#7994);
#7076=AXIS2_PLACEMENT_3D('',#10144,#7998,#7999);
#7077=AXIS2_PLACEMENT_3D('',#10147,#8002,#8003);
#7078=AXIS2_PLACEMENT_3D('',#10148,#8004,#8005);
#7079=AXIS2_PLACEMENT_3D('',#10149,#8006,#8007);
#7080=AXIS2_PLACEMENT_3D('',#10150,#8008,#8009);
#7081=AXIS2_PLACEMENT_3D('',#10159,#8014,#8015);
#7082=AXIS2_PLACEMENT_3D('',#10165,#8019,#8020);
#7083=AXIS2_PLACEMENT_3D('',#10171,#8024,#8025);
#7084=AXIS2_PLACEMENT_3D('',#10174,#8028,#8029);
#7085=AXIS2_PLACEMENT_3D('',#10175,#8030,#8031);
#7086=AXIS2_PLACEMENT_3D('',#10176,#8032,#8033);
#7087=AXIS2_PLACEMENT_3D('',#10177,#8034,#8035);
#7088=AXIS2_PLACEMENT_3D('',#10179,#8036,#8037);
#7089=AXIS2_PLACEMENT_3D('',#10182,#8039,#8040);
#7090=AXIS2_PLACEMENT_3D('',#10183,#8041,#8042);
#7091=AXIS2_PLACEMENT_3D('',#10185,#8043,#8044);
#7092=AXIS2_PLACEMENT_3D('',#10188,#8046,#8047);
#7093=AXIS2_PLACEMENT_3D('',#10189,#8048,#8049);
#7094=AXIS2_PLACEMENT_3D('',#10190,#8050,#8051);
#7095=AXIS2_PLACEMENT_3D('',#10192,#8052,#8053);
#7096=AXIS2_PLACEMENT_3D('',#10195,#8055,#8056);
#7097=AXIS2_PLACEMENT_3D('',#10196,#8057,#8058);
#7098=AXIS2_PLACEMENT_3D('',#10197,#8059,#8060);
#7099=AXIS2_PLACEMENT_3D('',#10199,#8061,#8062);
#7100=AXIS2_PLACEMENT_3D('',#10202,#8064,#8065);
#7101=AXIS2_PLACEMENT_3D('',#10203,#8066,#8067);
#7102=AXIS2_PLACEMENT_3D('',#10204,#8068,#8069);
#7103=AXIS2_PLACEMENT_3D('',#10206,#8070,#8071);
#7104=AXIS2_PLACEMENT_3D('',#10209,#8073,#8074);
#7105=AXIS2_PLACEMENT_3D('',#10210,#8075,#8076);
#7106=AXIS2_PLACEMENT_3D('',#10211,#8077,#8078);
#7107=AXIS2_PLACEMENT_3D('',#10213,#8079,#8080);
#7108=AXIS2_PLACEMENT_3D('',#10216,#8082,#8083);
#7109=AXIS2_PLACEMENT_3D('',#10217,#8084,#8085);
#7110=AXIS2_PLACEMENT_3D('',#10219,#8086,#8087);
#7111=AXIS2_PLACEMENT_3D('',#10222,#8089,#8090);
#7112=AXIS2_PLACEMENT_3D('',#10223,#8091,#8092);
#7113=AXIS2_PLACEMENT_3D('',#10225,#8093,#8094);
#7114=AXIS2_PLACEMENT_3D('',#10228,#8096,#8097);
#7115=AXIS2_PLACEMENT_3D('',#10229,#8098,#8099);
#7116=AXIS2_PLACEMENT_3D('',#10231,#8100,#8101);
#7117=AXIS2_PLACEMENT_3D('',#10234,#8103,#8104);
#7118=AXIS2_PLACEMENT_3D('',#10235,#8105,#8106);
#7119=AXIS2_PLACEMENT_3D('',#10237,#8107,#8108);
#7120=AXIS2_PLACEMENT_3D('',#10240,#8110,#8111);
#7121=AXIS2_PLACEMENT_3D('',#10241,#8112,#8113);
#7122=AXIS2_PLACEMENT_3D('',#10243,#8114,#8115);
#7123=AXIS2_PLACEMENT_3D('',#10246,#8117,#8118);
#7124=AXIS2_PLACEMENT_3D('',#10247,#8119,#8120);
#7125=AXIS2_PLACEMENT_3D('',#10249,#8121,#8122);
#7126=AXIS2_PLACEMENT_3D('',#10252,#8124,#8125);
#7127=AXIS2_PLACEMENT_3D('',#10253,#8126,#8127);
#7128=AXIS2_PLACEMENT_3D('',#10255,#8128,#8129);
#7129=AXIS2_PLACEMENT_3D('',#10258,#8131,#8132);
#7130=AXIS2_PLACEMENT_3D('',#10259,#8133,#8134);
#7131=AXIS2_PLACEMENT_3D('',#10261,#8135,#8136);
#7132=AXIS2_PLACEMENT_3D('',#10264,#8138,#8139);
#7133=AXIS2_PLACEMENT_3D('',#10265,#8140,#8141);
#7134=AXIS2_PLACEMENT_3D('',#10267,#8142,#8143);
#7135=AXIS2_PLACEMENT_3D('',#10268,#8144,#8145);
#7136=AXIS2_PLACEMENT_3D('',#10270,#8146,#8147);
#7137=AXIS2_PLACEMENT_3D('',#10272,#8149,#8150);
#7138=AXIS2_PLACEMENT_3D('',#10274,#8151,#8152);
#7139=AXIS2_PLACEMENT_3D('',#10277,#8154,#8155);
#7140=AXIS2_PLACEMENT_3D('',#10278,#8156,#8157);
#7141=AXIS2_PLACEMENT_3D('',#10283,#8159,#8160);
#7142=AXIS2_PLACEMENT_3D('',#10286,#8162,#8163);
#7143=AXIS2_PLACEMENT_3D('',#10287,#8164,#8165);
#7144=AXIS2_PLACEMENT_3D('',#10303,#8173,#8174);
#7145=AXIS2_PLACEMENT_3D('',#10305,#8176,#8177);
#7146=AXIS2_PLACEMENT_3D('',#10309,#8180,#8181);
#7147=AXIS2_PLACEMENT_3D('',#10323,#8189,#8190);
#7148=AXIS2_PLACEMENT_3D('',#10329,#8194,#8195);
#7149=AXIS2_PLACEMENT_3D('',#10333,#8198,#8199);
#7150=AXIS2_PLACEMENT_3D('',#10337,#8202,#8203);
#7151=AXIS2_PLACEMENT_3D('',#10339,#8205,#8206);
#7152=AXIS2_PLACEMENT_3D('',#10343,#8209,#8210);
#7153=AXIS2_PLACEMENT_3D('',#10348,#8213,#8214);
#7154=AXIS2_PLACEMENT_3D('',#10349,#8215,#8216);
#7155=AXIS2_PLACEMENT_3D('',#10357,#8222,#8223);
#7156=AXIS2_PLACEMENT_3D('',#10358,#8224,#8225);
#7157=AXIS2_PLACEMENT_3D('',#10359,#8226,#8227);
#7158=AXIS2_PLACEMENT_3D('',#10361,#8229,#8230);
#7159=AXIS2_PLACEMENT_3D('',#10363,#8232,#8233);
#7160=AXIS2_PLACEMENT_3D('',#10364,#8234,#8235);
#7161=AXIS2_PLACEMENT_3D('',#10365,#8236,#8237);
#7162=AXIS2_PLACEMENT_3D('',#10366,#8238,#8239);
#7163=AXIS2_PLACEMENT_3D('',#10368,#8240,#8241);
#7164=AXIS2_PLACEMENT_3D('',#10371,#8243,#8244);
#7165=AXIS2_PLACEMENT_3D('',#10372,#8245,#8246);
#7166=AXIS2_PLACEMENT_3D('',#10374,#8247,#8248);
#7167=AXIS2_PLACEMENT_3D('',#10377,#8250,#8251);
#7168=AXIS2_PLACEMENT_3D('',#10378,#8252,#8253);
#7169=AXIS2_PLACEMENT_3D('',#10380,#8254,#8255);
#7170=AXIS2_PLACEMENT_3D('',#10383,#8257,#8258);
#7171=AXIS2_PLACEMENT_3D('',#10384,#8259,#8260);
#7172=AXIS2_PLACEMENT_3D('',#10386,#8261,#8262);
#7173=AXIS2_PLACEMENT_3D('',#10389,#8264,#8265);
#7174=AXIS2_PLACEMENT_3D('',#10390,#8266,#8267);
#7175=AXIS2_PLACEMENT_3D('',#10392,#8268,#8269);
#7176=AXIS2_PLACEMENT_3D('',#10395,#8271,#8272);
#7177=AXIS2_PLACEMENT_3D('',#10396,#8273,#8274);
#7178=AXIS2_PLACEMENT_3D('',#10398,#8275,#8276);
#7179=AXIS2_PLACEMENT_3D('',#10399,#8277,#8278);
#7180=AXIS2_PLACEMENT_3D('',#10402,#8280,#8281);
#7181=AXIS2_PLACEMENT_3D('',#10403,#8282,#8283);
#7182=AXIS2_PLACEMENT_3D('',#10405,#8284,#8285);
#7183=AXIS2_PLACEMENT_3D('',#10408,#8287,#8288);
#7184=AXIS2_PLACEMENT_3D('',#10409,#8289,#8290);
#7185=AXIS2_PLACEMENT_3D('',#10410,#8291,#8292);
#7186=AXIS2_PLACEMENT_3D('',#10411,#8293,#8294);
#7187=AXIS2_PLACEMENT_3D('',#10412,#8295,#8296);
#7188=AXIS2_PLACEMENT_3D('',#10414,#8297,#8298);
#7189=AXIS2_PLACEMENT_3D('',#10417,#8300,#8301);
#7190=AXIS2_PLACEMENT_3D('',#10418,#8302,#8303);
#7191=AXIS2_PLACEMENT_3D('',#10420,#8304,#8305);
#7192=AXIS2_PLACEMENT_3D('',#10423,#8307,#8308);
#7193=AXIS2_PLACEMENT_3D('',#10424,#8309,#8310);
#7194=AXIS2_PLACEMENT_3D('',#10426,#8311,#8312);
#7195=AXIS2_PLACEMENT_3D('',#10429,#8314,#8315);
#7196=AXIS2_PLACEMENT_3D('',#10430,#8316,#8317);
#7197=AXIS2_PLACEMENT_3D('',#10432,#8318,#8319);
#7198=AXIS2_PLACEMENT_3D('',#10435,#8321,#8322);
#7199=AXIS2_PLACEMENT_3D('',#10436,#8323,#8324);
#7200=AXIS2_PLACEMENT_3D('',#10438,#8325,#8326);
#7201=AXIS2_PLACEMENT_3D('',#10441,#8328,#8329);
#7202=AXIS2_PLACEMENT_3D('',#10442,#8330,#8331);
#7203=AXIS2_PLACEMENT_3D('',#10444,#8332,#8333);
#7204=AXIS2_PLACEMENT_3D('',#10445,#8334,#8335);
#7205=AXIS2_PLACEMENT_3D('',#10447,#8336,#8337);
#7206=AXIS2_PLACEMENT_3D('',#10449,#8339,#8340);
#7207=AXIS2_PLACEMENT_3D('',#10451,#8341,#8342);
#7208=AXIS2_PLACEMENT_3D('',#10454,#8344,#8345);
#7209=AXIS2_PLACEMENT_3D('',#10455,#8346,#8347);
#7210=AXIS2_PLACEMENT_3D('',#10456,#8348,#8349);
#7211=AXIS2_PLACEMENT_3D('',#10457,#8350,#8351);
#7212=AXIS2_PLACEMENT_3D('',#10458,#8352,#8353);
#7213=AXIS2_PLACEMENT_3D('',#10460,#8354,#8355);
#7214=AXIS2_PLACEMENT_3D('',#10463,#8357,#8358);
#7215=AXIS2_PLACEMENT_3D('',#10464,#8359,#8360);
#7216=AXIS2_PLACEMENT_3D('',#10466,#8361,#8362);
#7217=AXIS2_PLACEMENT_3D('',#10467,#8363,#8364);
#7218=AXIS2_PLACEMENT_3D('',#10469,#8365,#8366);
#7219=AXIS2_PLACEMENT_3D('',#10472,#8368,#8369);
#7220=AXIS2_PLACEMENT_3D('',#10473,#8370,#8371);
#7221=AXIS2_PLACEMENT_3D('',#10475,#8372,#8373);
#7222=AXIS2_PLACEMENT_3D('',#10476,#8374,#8375);
#7223=AXIS2_PLACEMENT_3D('',#10478,#8376,#8377);
#7224=AXIS2_PLACEMENT_3D('',#10481,#8379,#8380);
#7225=AXIS2_PLACEMENT_3D('',#10482,#8381,#8382);
#7226=AXIS2_PLACEMENT_3D('',#10484,#8383,#8384);
#7227=AXIS2_PLACEMENT_3D('',#10485,#8385,#8386);
#7228=AXIS2_PLACEMENT_3D('',#10487,#8387,#8388);
#7229=AXIS2_PLACEMENT_3D('',#10490,#8390,#8391);
#7230=AXIS2_PLACEMENT_3D('',#10491,#8392,#8393);
#7231=AXIS2_PLACEMENT_3D('',#10493,#8394,#8395);
#7232=AXIS2_PLACEMENT_3D('',#10494,#8396,#8397);
#7233=AXIS2_PLACEMENT_3D('',#10496,#8398,#8399);
#7234=AXIS2_PLACEMENT_3D('',#10498,#8401,#8402);
#7235=AXIS2_PLACEMENT_3D('',#10500,#8403,#8404);
#7236=AXIS2_PLACEMENT_3D('',#10502,#8406,#8407);
#7237=AXIS2_PLACEMENT_3D('',#10504,#8408,#8409);
#7238=AXIS2_PLACEMENT_3D('',#10506,#8411,#8412);
#7239=AXIS2_PLACEMENT_3D('',#10508,#8413,#8414);
#7240=AXIS2_PLACEMENT_3D('',#10510,#8416,#8417);
#7241=AXIS2_PLACEMENT_3D('',#10512,#8418,#8419);
#7242=AXIS2_PLACEMENT_3D('',#10515,#8421,#8422);
#7243=AXIS2_PLACEMENT_3D('',#10516,#8423,#8424);
#7244=AXIS2_PLACEMENT_3D('',#10518,#8425,#8426);
#7245=AXIS2_PLACEMENT_3D('',#10519,#8427,#8428);
#7246=AXIS2_PLACEMENT_3D('',#10521,#8429,#8430);
#7247=AXIS2_PLACEMENT_3D('',#10523,#8432,#8433);
#7248=AXIS2_PLACEMENT_3D('',#10525,#8434,#8435);
#7249=AXIS2_PLACEMENT_3D('',#10528,#8437,#8438);
#7250=AXIS2_PLACEMENT_3D('',#10529,#8439,#8440);
#7251=AXIS2_PLACEMENT_3D('',#10530,#8441,#8442);
#7252=AXIS2_PLACEMENT_3D('',#10531,#8443,#8444);
#7253=AXIS2_PLACEMENT_3D('',#10532,#8445,#8446);
#7254=AXIS2_PLACEMENT_3D('',#10541,#8451,#8452);
#7255=AXIS2_PLACEMENT_3D('',#10547,#8456,#8457);
#7256=AXIS2_PLACEMENT_3D('',#10553,#8461,#8462);
#7257=AXIS2_PLACEMENT_3D('',#10556,#8465,#8466);
#7258=AXIS2_PLACEMENT_3D('',#10557,#8467,#8468);
#7259=AXIS2_PLACEMENT_3D('',#10558,#8469,#8470);
#7260=AXIS2_PLACEMENT_3D('',#10559,#8471,#8472);
#7261=AXIS2_PLACEMENT_3D('',#10561,#8473,#8474);
#7262=AXIS2_PLACEMENT_3D('',#10564,#8476,#8477);
#7263=AXIS2_PLACEMENT_3D('',#10565,#8478,#8479);
#7264=AXIS2_PLACEMENT_3D('',#10566,#8480,#8481);
#7265=AXIS2_PLACEMENT_3D('',#10568,#8482,#8483);
#7266=AXIS2_PLACEMENT_3D('',#10571,#8485,#8486);
#7267=AXIS2_PLACEMENT_3D('',#10572,#8487,#8488);
#7268=AXIS2_PLACEMENT_3D('',#10573,#8489,#8490);
#7269=AXIS2_PLACEMENT_3D('',#10582,#8495,#8496);
#7270=AXIS2_PLACEMENT_3D('',#10588,#8500,#8501);
#7271=AXIS2_PLACEMENT_3D('',#10594,#8505,#8506);
#7272=AXIS2_PLACEMENT_3D('',#10597,#8509,#8510);
#7273=AXIS2_PLACEMENT_3D('',#10598,#8511,#8512);
#7274=AXIS2_PLACEMENT_3D('',#10599,#8513,#8514);
#7275=AXIS2_PLACEMENT_3D('',#10600,#8515,#8516);
#7276=AXIS2_PLACEMENT_3D('',#10602,#8517,#8518);
#7277=AXIS2_PLACEMENT_3D('',#10605,#8520,#8521);
#7278=AXIS2_PLACEMENT_3D('',#10606,#8522,#8523);
#7279=AXIS2_PLACEMENT_3D('',#10607,#8524,#8525);
#7280=AXIS2_PLACEMENT_3D('',#10609,#8526,#8527);
#7281=AXIS2_PLACEMENT_3D('',#10612,#8529,#8530);
#7282=AXIS2_PLACEMENT_3D('',#10613,#8531,#8532);
#7283=AXIS2_PLACEMENT_3D('',#10614,#8533,#8534);
#7284=AXIS2_PLACEMENT_3D('',#10623,#8539,#8540);
#7285=AXIS2_PLACEMENT_3D('',#10629,#8544,#8545);
#7286=AXIS2_PLACEMENT_3D('',#10635,#8549,#8550);
#7287=AXIS2_PLACEMENT_3D('',#10638,#8553,#8554);
#7288=AXIS2_PLACEMENT_3D('',#10639,#8555,#8556);
#7289=AXIS2_PLACEMENT_3D('',#10640,#8557,#8558);
#7290=AXIS2_PLACEMENT_3D('',#10641,#8559,#8560);
#7291=AXIS2_PLACEMENT_3D('',#10643,#8561,#8562);
#7292=AXIS2_PLACEMENT_3D('',#10646,#8564,#8565);
#7293=AXIS2_PLACEMENT_3D('',#10647,#8566,#8567);
#7294=AXIS2_PLACEMENT_3D('',#10648,#8568,#8569);
#7295=AXIS2_PLACEMENT_3D('',#10650,#8570,#8571);
#7296=AXIS2_PLACEMENT_3D('',#10652,#8572,#8573);
#7297=AXIS2_PLACEMENT_3D('',#10653,#8574,#8575);
#7298=AXIS2_PLACEMENT_3D('',#10655,#8576,#8577);
#7299=AXIS2_PLACEMENT_3D('',#10657,#8579,#8580);
#7300=AXIS2_PLACEMENT_3D('',#10658,#8581,#8582);
#7301=AXIS2_PLACEMENT_3D('',#10661,#8584,#8585);
#7302=AXIS2_PLACEMENT_3D('',#10662,#8586,#8587);
#7303=AXIS2_PLACEMENT_3D('',#10663,#8588,#8589);
#7304=AXIS2_PLACEMENT_3D('',#10664,#8590,#8591);
#7305=AXIS2_PLACEMENT_3D('',#10673,#8596,#8597);
#7306=AXIS2_PLACEMENT_3D('',#10679,#8601,#8602);
#7307=AXIS2_PLACEMENT_3D('',#10685,#8606,#8607);
#7308=AXIS2_PLACEMENT_3D('',#10691,#8611,#8612);
#7309=AXIS2_PLACEMENT_3D('',#10697,#8616,#8617);
#7310=AXIS2_PLACEMENT_3D('',#10700,#8620,#8621);
#7311=AXIS2_PLACEMENT_3D('',#10701,#8622,#8623);
#7312=AXIS2_PLACEMENT_3D('',#10702,#8624,#8625);
#7313=AXIS2_PLACEMENT_3D('',#10704,#8626,#8627);
#7314=AXIS2_PLACEMENT_3D('',#10705,#8628,#8629);
#7315=AXIS2_PLACEMENT_3D('',#10707,#8630,#8631);
#7316=AXIS2_PLACEMENT_3D('',#10708,#8632,#8633);
#7317=AXIS2_PLACEMENT_3D('',#10710,#8634,#8635);
#7318=AXIS2_PLACEMENT_3D('',#10712,#8637,#8638);
#7319=AXIS2_PLACEMENT_3D('',#10714,#8639,#8640);
#7320=AXIS2_PLACEMENT_3D('',#10716,#8642,#8643);
#7321=AXIS2_PLACEMENT_3D('',#10718,#8644,#8645);
#7322=AXIS2_PLACEMENT_3D('',#10720,#8647,#8648);
#7323=AXIS2_PLACEMENT_3D('',#10722,#8649,#8650);
#7324=AXIS2_PLACEMENT_3D('',#10723,#8651,#8652);
#7325=AXIS2_PLACEMENT_3D('',#10725,#8653,#8654);
#7326=AXIS2_PLACEMENT_3D('',#10727,#8656,#8657);
#7327=AXIS2_PLACEMENT_3D('',#10729,#8659,#8660);
#7328=AXIS2_PLACEMENT_3D('',#10730,#8661,#8662);
#7329=AXIS2_PLACEMENT_3D('',#10731,#8663,#8664);
#7330=AXIS2_PLACEMENT_3D('',#10734,#8665,#8666);
#7331=AXIS2_PLACEMENT_3D('',#10735,#8667,#8668);
#7332=AXIS2_PLACEMENT_3D('',#10737,#8669,#8670);
#7333=AXIS2_PLACEMENT_3D('',#10739,#8671,#8672);
#7334=AXIS2_PLACEMENT_3D('',#10740,#8673,#8674);
#7335=AXIS2_PLACEMENT_3D('',#10741,#8675,#8676);
#7336=AXIS2_PLACEMENT_3D('',#10744,#8678,#8679);
#7337=AXIS2_PLACEMENT_3D('',#10745,#8680,#8681);
#7338=AXIS2_PLACEMENT_3D('',#10747,#8682,#8683);
#7339=AXIS2_PLACEMENT_3D('',#10750,#8685,#8686);
#7340=AXIS2_PLACEMENT_3D('',#10751,#8687,#8688);
#7341=AXIS2_PLACEMENT_3D('',#10754,#8690,#8691);
#7342=AXIS2_PLACEMENT_3D('',#10755,#8692,#8693);
#7343=AXIS2_PLACEMENT_3D('',#10756,#8694,#8695);
#7344=AXIS2_PLACEMENT_3D('',#10758,#8696,#8697);
#7345=AXIS2_PLACEMENT_3D('',#10760,#8699,#8700);
#7346=AXIS2_PLACEMENT_3D('',#10762,#8701,#8702);
#7347=AXIS2_PLACEMENT_3D('',#10763,#8703,#8704);
#7348=AXIS2_PLACEMENT_3D('',#10765,#8706,#8707);
#7349=AXIS2_PLACEMENT_3D('',#10766,#8708,#8709);
#7350=AXIS2_PLACEMENT_3D('',#10769,#8710,#8711);
#7351=AXIS2_PLACEMENT_3D('',#10770,#8712,#8713);
#7352=AXIS2_PLACEMENT_3D('',#10772,#8714,#8715);
#7353=AXIS2_PLACEMENT_3D('',#10774,#8716,#8717);
#7354=AXIS2_PLACEMENT_3D('',#10775,#8718,#8719);
#7355=AXIS2_PLACEMENT_3D('',#10776,#8720,#8721);
#7356=AXIS2_PLACEMENT_3D('',#10778,#8722,#8723);
#7357=AXIS2_PLACEMENT_3D('',#10780,#8725,#8726);
#7358=AXIS2_PLACEMENT_3D('',#10782,#8727,#8728);
#7359=AXIS2_PLACEMENT_3D('',#10784,#8729,#8730);
#7360=AXIS2_PLACEMENT_3D('',#10785,#8731,#8732);
#7361=AXIS2_PLACEMENT_3D('',#10787,#8733,#8734);
#7362=AXIS2_PLACEMENT_3D('',#10789,#8736,#8737);
#7363=AXIS2_PLACEMENT_3D('',#10791,#8738,#8739);
#7364=AXIS2_PLACEMENT_3D('',#10793,#8741,#8742);
#7365=AXIS2_PLACEMENT_3D('',#10795,#8743,#8744);
#7366=AXIS2_PLACEMENT_3D('',#10797,#8746,#8747);
#7367=AXIS2_PLACEMENT_3D('',#10798,#8748,#8749);
#7368=AXIS2_PLACEMENT_3D('',#10800,#8751,#8752);
#7369=AXIS2_PLACEMENT_3D('',#10801,#8753,#8754);
#7370=AXIS2_PLACEMENT_3D('',#10804,#8755,#8756);
#7371=AXIS2_PLACEMENT_3D('',#10805,#8757,#8758);
#7372=AXIS2_PLACEMENT_3D('',#10808,#8759,#8760);
#7373=AXIS2_PLACEMENT_3D('',#10809,#8761,#8762);
#7374=AXIS2_PLACEMENT_3D('',#10812,#8763,#8764);
#7375=AXIS2_PLACEMENT_3D('',#10813,#8765,#8766);
#7376=AXIS2_PLACEMENT_3D('',#10816,#8767,#8768);
#7377=AXIS2_PLACEMENT_3D('',#10817,#8769,#8770);
#7378=AXIS2_PLACEMENT_3D('',#10820,#8771,#8772);
#7379=AXIS2_PLACEMENT_3D('',#10821,#8773,#8774);
#7380=AXIS2_PLACEMENT_3D('',#10824,#8775,#8776);
#7381=AXIS2_PLACEMENT_3D('',#10825,#8777,#8778);
#7382=AXIS2_PLACEMENT_3D('',#10828,#8779,#8780);
#7383=AXIS2_PLACEMENT_3D('',#10829,#8781,#8782);
#7384=AXIS2_PLACEMENT_3D('',#10832,#8783,#8784);
#7385=AXIS2_PLACEMENT_3D('',#10833,#8785,#8786);
#7386=AXIS2_PLACEMENT_3D('',#10834,#8787,#8788);
#7387=AXIS2_PLACEMENT_3D('',#10860,#8789,#8790);
#7388=AXIS2_PLACEMENT_3D('',#10884,#8791,#8792);
#7389=AXIS2_PLACEMENT_3D('',#10885,#8793,#8794);
#7390=AXIS2_PLACEMENT_3D('',#10887,#8795,#8796);
#7391=AXIS2_PLACEMENT_3D('',#10912,#8797,#8798);
#7392=AXIS2_PLACEMENT_3D('',#10937,#8799,#8800);
#7393=AXIS2_PLACEMENT_3D('',#10953,#8802,#8803);
#7394=AXIS2_PLACEMENT_3D('',#10968,#8804,#8805);
#7395=AXIS2_PLACEMENT_3D('',#10993,#8806,#8807);
#7396=AXIS2_PLACEMENT_3D('',#11018,#8808,#8809);
#7397=AXIS2_PLACEMENT_3D('',#11043,#8810,#8811);
#7398=AXIS2_PLACEMENT_3D('',#11067,#8812,#8813);
#7399=AXIS2_PLACEMENT_3D('',#11068,#8814,#8815);
#7400=AXIS2_PLACEMENT_3D('',#11070,#8816,#8817);
#7401=AXIS2_PLACEMENT_3D('',#11071,#8818,#8819);
#7402=AXIS2_PLACEMENT_3D('',#11072,#8820,#8821);
#7403=AXIS2_PLACEMENT_3D('',#11096,#8822,#8823);
#7404=AXIS2_PLACEMENT_3D('',#11097,#8824,#8825);
#7405=AXIS2_PLACEMENT_3D('',#11099,#8826,#8827);
#7406=AXIS2_PLACEMENT_3D('',#11100,#8828,#8829);
#7407=AXIS2_PLACEMENT_3D('',#11101,#8830,#8831);
#7408=AXIS2_PLACEMENT_3D('',#11125,#8832,#8833);
#7409=AXIS2_PLACEMENT_3D('',#11126,#8834,#8835);
#7410=AXIS2_PLACEMENT_3D('',#11128,#8836,#8837);
#7411=AXIS2_PLACEMENT_3D('',#11129,#8838,#8839);
#7412=AXIS2_PLACEMENT_3D('',#11130,#8840,#8841);
#7413=AXIS2_PLACEMENT_3D('',#11145,#8842,#8843);
#7414=AXIS2_PLACEMENT_3D('',#11158,#8844,#8845);
#7415=AXIS2_PLACEMENT_3D('',#11160,#8846,#8847);
#7416=AXIS2_PLACEMENT_3D('',#11161,#8848,#8849);
#7417=AXIS2_PLACEMENT_3D('',#11162,#8850,#8851);
#7418=AXIS2_PLACEMENT_3D('',#11186,#8852,#8853);
#7419=AXIS2_PLACEMENT_3D('',#11187,#8854,#8855);
#7420=AXIS2_PLACEMENT_3D('',#11189,#8856,#8857);
#7421=AXIS2_PLACEMENT_3D('',#11190,#8858,#8859);
#7422=AXIS2_PLACEMENT_3D('',#11191,#8860,#8861);
#7423=AXIS2_PLACEMENT_3D('',#11215,#8862,#8863);
#7424=AXIS2_PLACEMENT_3D('',#11216,#8864,#8865);
#7425=AXIS2_PLACEMENT_3D('',#11218,#8866,#8867);
#7426=AXIS2_PLACEMENT_3D('',#11219,#8868,#8869);
#7427=AXIS2_PLACEMENT_3D('',#11220,#8870,#8871);
#7428=AXIS2_PLACEMENT_3D('',#11244,#8872,#8873);
#7429=AXIS2_PLACEMENT_3D('',#11245,#8874,#8875);
#7430=AXIS2_PLACEMENT_3D('',#11247,#8876,#8877);
#7431=AXIS2_PLACEMENT_3D('',#11250,#8879,#8880);
#7432=AXIS2_PLACEMENT_3D('',#11274,#8881,#8882);
#7433=AXIS2_PLACEMENT_3D('',#11275,#8883,#8884);
#7434=AXIS2_PLACEMENT_3D('',#11276,#8885,#8886);
#7435=AXIS2_PLACEMENT_3D('',#11277,#8887,#8888);
#7436=AXIS2_PLACEMENT_3D('',#11278,#8889,#8890);
#7437=AXIS2_PLACEMENT_3D('',#11279,#8891,#8892);
#7438=AXIS2_PLACEMENT_3D('',#11280,#8893,#8894);
#7439=AXIS2_PLACEMENT_3D('',#11281,#8895,#8896);
#7440=AXIS2_PLACEMENT_3D('',#11282,#8897,#8898);
#7441=AXIS2_PLACEMENT_3D('',#11284,#8899,#8900);
#7442=AXIS2_PLACEMENT_3D('',#11286,#8901,#8902);
#7443=AXIS2_PLACEMENT_3D('',#11287,#8903,#8904);
#7444=AXIS2_PLACEMENT_3D('',#11289,#8905,#8906);
#7445=AXIS2_PLACEMENT_3D('',#11291,#8908,#8909);
#7446=AXIS2_PLACEMENT_3D('',#11293,#8910,#8911);
#7447=AXIS2_PLACEMENT_3D('',#11294,#8912,#8913);
#7448=AXIS2_PLACEMENT_3D('',#11296,#8915,#8916);
#7449=AXIS2_PLACEMENT_3D('',#11298,#8917,#8918);
#7450=AXIS2_PLACEMENT_3D('',#11300,#8919,#8920);
#7451=AXIS2_PLACEMENT_3D('',#11301,#8921,#8922);
#7452=AXIS2_PLACEMENT_3D('',#11303,#8923,#8924);
#7453=AXIS2_PLACEMENT_3D('',#11305,#8926,#8927);
#7454=AXIS2_PLACEMENT_3D('',#11307,#8928,#8929);
#7455=AXIS2_PLACEMENT_3D('',#11308,#8930,#8931);
#7456=AXIS2_PLACEMENT_3D('',#11310,#8933,#8934);
#7457=AXIS2_PLACEMENT_3D('',#11311,#8935,#8936);
#7458=AXIS2_PLACEMENT_3D('',#11312,#8937,#8938);
#7459=AXIS2_PLACEMENT_3D('',#11313,#8939,#8940);
#7460=AXIS2_PLACEMENT_3D('',#11314,#8941,#8942);
#7461=AXIS2_PLACEMENT_3D('',#11315,#8943,#8944);
#7462=AXIS2_PLACEMENT_3D('',#11316,#8945,#8946);
#7463=AXIS2_PLACEMENT_3D('',#11317,#8947,#8948);
#7464=AXIS2_PLACEMENT_3D('',#11320,#8949,#8950);
#7465=AXIS2_PLACEMENT_3D('',#11326,#8954,#8955);
#7466=AXIS2_PLACEMENT_3D('',#11332,#8959,#8960);
#7467=AXIS2_PLACEMENT_3D('',#11334,#8961,#8962);
#7468=AXIS2_PLACEMENT_3D('',#11338,#8965,#8966);
#7469=AXIS2_PLACEMENT_3D('',#11341,#8969,#8970);
#7470=AXIS2_PLACEMENT_3D('',#11342,#8971,#8972);
#7471=AXIS2_PLACEMENT_3D('',#11344,#8973,#8974);
#7472=AXIS2_PLACEMENT_3D('',#11346,#8975,#8976);
#7473=AXIS2_PLACEMENT_3D('',#11347,#8977,#8978);
#7474=AXIS2_PLACEMENT_3D('',#11349,#8979,#8980);
#7475=AXIS2_PLACEMENT_3D('',#11351,#8982,#8983);
#7476=AXIS2_PLACEMENT_3D('',#11353,#8984,#8985);
#7477=AXIS2_PLACEMENT_3D('',#11354,#8986,#8987);
#7478=AXIS2_PLACEMENT_3D('',#11356,#8988,#8989);
#7479=AXIS2_PLACEMENT_3D('',#11358,#8991,#8992);
#7480=AXIS2_PLACEMENT_3D('',#11360,#8993,#8994);
#7481=AXIS2_PLACEMENT_3D('',#11361,#8995,#8996);
#7482=AXIS2_PLACEMENT_3D('',#11363,#8997,#8998);
#7483=AXIS2_PLACEMENT_3D('',#11365,#9000,#9001);
#7484=AXIS2_PLACEMENT_3D('',#11367,#9002,#9003);
#7485=AXIS2_PLACEMENT_3D('',#11368,#9004,#9005);
#7486=AXIS2_PLACEMENT_3D('',#11370,#9006,#9007);
#7487=AXIS2_PLACEMENT_3D('',#11372,#9009,#9010);
#7488=AXIS2_PLACEMENT_3D('',#11374,#9011,#9012);
#7489=AXIS2_PLACEMENT_3D('',#11375,#9013,#9014);
#7490=AXIS2_PLACEMENT_3D('',#11377,#9015,#9016);
#7491=AXIS2_PLACEMENT_3D('',#11379,#9018,#9019);
#7492=AXIS2_PLACEMENT_3D('',#11381,#9020,#9021);
#7493=AXIS2_PLACEMENT_3D('',#11382,#9022,#9023);
#7494=AXIS2_PLACEMENT_3D('',#11384,#9025,#9026);
#7495=AXIS2_PLACEMENT_3D('',#11385,#9027,#9028);
#7496=AXIS2_PLACEMENT_3D('',#11388,#9029,#9030);
#7497=AXIS2_PLACEMENT_3D('',#11392,#9032,#9033);
#7498=AXIS2_PLACEMENT_3D('',#11394,#9035,#9036);
#7499=AXIS2_PLACEMENT_3D('',#11400,#9040,#9041);
#7500=AXIS2_PLACEMENT_3D('',#11402,#9042,#9043);
#7501=AXIS2_PLACEMENT_3D('',#11404,#9044,#9045);
#7502=AXIS2_PLACEMENT_3D('',#11406,#9047,#9048);
#7503=AXIS2_PLACEMENT_3D('',#11409,#9051,#9052);
#7504=AXIS2_PLACEMENT_3D('',#11411,#9053,#9054);
#7505=AXIS2_PLACEMENT_3D('',#11413,#9055,#9056);
#7506=AXIS2_PLACEMENT_3D('',#11414,#9057,#9058);
#7507=AXIS2_PLACEMENT_3D('',#11416,#9059,#9060);
#7508=AXIS2_PLACEMENT_3D('',#11418,#9062,#9063);
#7509=AXIS2_PLACEMENT_3D('',#11420,#9064,#9065);
#7510=AXIS2_PLACEMENT_3D('',#11421,#9066,#9067);
#7511=AXIS2_PLACEMENT_3D('',#11423,#9069,#9070);
#7512=AXIS2_PLACEMENT_3D('',#11424,#9071,#9072);
#7513=AXIS2_PLACEMENT_3D('',#11425,#9073,#9074);
#7514=AXIS2_PLACEMENT_3D('',#11426,#9075,#9076);
#7515=AXIS2_PLACEMENT_3D('',#11435,#9081,#9082);
#7516=AXIS2_PLACEMENT_3D('',#11441,#9086,#9087);
#7517=AXIS2_PLACEMENT_3D('',#11447,#9091,#9092);
#7518=AXIS2_PLACEMENT_3D('',#11453,#9096,#9097);
#7519=AXIS2_PLACEMENT_3D('',#11459,#9101,#9102);
#7520=AXIS2_PLACEMENT_3D('',#11462,#9105,#9106);
#7521=AXIS2_PLACEMENT_3D('',#11463,#9107,#9108);
#7522=AXIS2_PLACEMENT_3D('',#11464,#9109,#9110);
#7523=AXIS2_PLACEMENT_3D('',#11466,#9111,#9112);
#7524=AXIS2_PLACEMENT_3D('',#11468,#9113,#9114);
#7525=AXIS2_PLACEMENT_3D('',#11469,#9115,#9116);
#7526=AXIS2_PLACEMENT_3D('',#11472,#9118,#9119);
#7527=AXIS2_PLACEMENT_3D('',#11473,#9120,#9121);
#7528=AXIS2_PLACEMENT_3D('',#11474,#9122,#9123);
#7529=AXIS2_PLACEMENT_3D('',#11476,#9124,#9125);
#7530=AXIS2_PLACEMENT_3D('',#11477,#9126,#9127);
#7531=AXIS2_PLACEMENT_3D('',#11479,#9128,#9129);
#7532=AXIS2_PLACEMENT_3D('',#11481,#9131,#9132);
#7533=AXIS2_PLACEMENT_3D('',#11483,#9133,#9134);
#7534=AXIS2_PLACEMENT_3D('',#11485,#9136,#9137);
#7535=AXIS2_PLACEMENT_3D('',#11487,#9138,#9139);
#7536=AXIS2_PLACEMENT_3D('',#11489,#9141,#9142);
#7537=AXIS2_PLACEMENT_3D('',#11491,#9143,#9144);
#7538=AXIS2_PLACEMENT_3D('',#11492,#9145,#9146);
#7539=AXIS2_PLACEMENT_3D('',#11494,#9147,#9148);
#7540=AXIS2_PLACEMENT_3D('',#11496,#9150,#9151);
#7541=AXIS2_PLACEMENT_3D('',#11498,#9152,#9153);
#7542=AXIS2_PLACEMENT_3D('',#11500,#9155,#9156);
#7543=AXIS2_PLACEMENT_3D('',#11502,#9158,#9159);
#7544=AXIS2_PLACEMENT_3D('',#11503,#9160,#9161);
#7545=AXIS2_PLACEMENT_3D('',#11504,#9162,#9163);
#7546=AXIS2_PLACEMENT_3D('',#11506,#9164,#9165);
#7547=AXIS2_PLACEMENT_3D('',#11509,#9167,#9168);
#7548=AXIS2_PLACEMENT_3D('',#11510,#9169,#9170);
#7549=AXIS2_PLACEMENT_3D('',#11515,#9172,#9173);
#7550=AXIS2_PLACEMENT_3D('',#11518,#9175,#9176);
#7551=AXIS2_PLACEMENT_3D('',#11519,#9177,#9178);
#7552=AXIS2_PLACEMENT_3D('',#11523,#9180,#9181);
#7553=AXIS2_PLACEMENT_3D('',#11525,#9182,#9183);
#7554=AXIS2_PLACEMENT_3D('',#11529,#9185,#9186);
#7555=AXIS2_PLACEMENT_3D('',#11533,#9188,#9189);
#7556=AXIS2_PLACEMENT_3D('',#11536,#9191,#9192);
#7557=AXIS2_PLACEMENT_3D('',#11537,#9193,#9194);
#7558=AXIS2_PLACEMENT_3D('',#11541,#9197,#9198);
#7559=AXIS2_PLACEMENT_3D('',#11544,#9200,#9201);
#7560=AXIS2_PLACEMENT_3D('',#11545,#9202,#9203);
#7561=AXIS2_PLACEMENT_3D('',#11547,#9205,#9206);
#7562=AXIS2_PLACEMENT_3D('',#11551,#9208,#9209);
#7563=AXIS2_PLACEMENT_3D('',#11553,#9211,#9212);
#7564=AXIS2_PLACEMENT_3D('',#11557,#9215,#9216);
#7565=AXIS2_PLACEMENT_3D('',#11560,#9218,#9219);
#7566=AXIS2_PLACEMENT_3D('',#11561,#9220,#9221);
#7567=AXIS2_PLACEMENT_3D('',#11563,#9223,#9224);
#7568=AXIS2_PLACEMENT_3D('',#11565,#9225,#9226);
#7569=AXIS2_PLACEMENT_3D('',#11567,#9227,#9228);
#7570=AXIS2_PLACEMENT_3D('',#11568,#9229,#9230);
#7571=AXIS2_PLACEMENT_3D('',#11570,#9232,#9233);
#7572=AXIS2_PLACEMENT_3D('',#11572,#9234,#9235);
#7573=AXIS2_PLACEMENT_3D('',#11574,#9236,#9237);
#7574=AXIS2_PLACEMENT_3D('',#11575,#9238,#9239);
#7575=AXIS2_PLACEMENT_3D('',#11577,#9241,#9242);
#7576=AXIS2_PLACEMENT_3D('',#11580,#9244,#9245);
#7577=AXIS2_PLACEMENT_3D('',#11581,#9246,#9247);
#7578=AXIS2_PLACEMENT_3D('',#11583,#9248,#9249);
#7579=AXIS2_PLACEMENT_3D('',#11585,#9251,#9252);
#7580=AXIS2_PLACEMENT_3D('',#11586,#9253,#9254);
#7581=AXIS2_PLACEMENT_3D('',#11587,#9255,#9256);
#7582=AXIS2_PLACEMENT_3D('',#11588,#9257,#9258);
#7583=AXIS2_PLACEMENT_3D('',#11590,#9259,#9260);
#7584=AXIS2_PLACEMENT_3D('',#11593,#9262,#9263);
#7585=AXIS2_PLACEMENT_3D('',#11594,#9264,#9265);
#7586=AXIS2_PLACEMENT_3D('',#11596,#9266,#9267);
#7587=AXIS2_PLACEMENT_3D('',#11599,#9269,#9270);
#7588=AXIS2_PLACEMENT_3D('',#11600,#9271,#9272);
#7589=AXIS2_PLACEMENT_3D('',#11601,#9273,#9274);
#7590=AXIS2_PLACEMENT_3D('',#11602,#9275,#9276);
#7591=AXIS2_PLACEMENT_3D('',#11603,#9277,#9278);
#7592=AXIS2_PLACEMENT_3D('',#11607,#9280,#9281);
#7593=AXIS2_PLACEMENT_3D('',#11608,#9282,#9283);
#7594=AXIS2_PLACEMENT_3D('',#11625,#9284,#9285);
#7595=AXIS2_PLACEMENT_3D('',#11666,#9287,#9288);
#7596=AXIS2_PLACEMENT_3D('',#11681,#9289,#9290);
#7597=AXIS2_PLACEMENT_3D('',#11683,#9292,#9293);
#7598=AXIS2_PLACEMENT_3D('',#11685,#9294,#9295);
#7599=AXIS2_PLACEMENT_3D('',#11688,#9297,#9298);
#7600=AXIS2_PLACEMENT_3D('',#11689,#9299,#9300);
#7601=AXIS2_PLACEMENT_3D('',#11691,#9301,#9302);
#7602=AXIS2_PLACEMENT_3D('',#11694,#9304,#9305);
#7603=AXIS2_PLACEMENT_3D('',#11695,#9306,#9307);
#7604=AXIS2_PLACEMENT_3D('',#11696,#9308,#9309);
#7605=AXIS2_PLACEMENT_3D('',#11697,#9310,#9311);
#7606=AXIS2_PLACEMENT_3D('',#11698,#9312,#9313);
#7607=AXIS2_PLACEMENT_3D('',#11700,#9314,#9315);
#7608=AXIS2_PLACEMENT_3D('',#11703,#9317,#9318);
#7609=AXIS2_PLACEMENT_3D('',#11704,#9319,#9320);
#7610=AXIS2_PLACEMENT_3D('',#11705,#9321,#9322);
#7611=AXIS2_PLACEMENT_3D('',#11707,#9323,#9324);
#7612=AXIS2_PLACEMENT_3D('',#11710,#9326,#9327);
#7613=AXIS2_PLACEMENT_3D('',#11711,#9328,#9329);
#7614=AXIS2_PLACEMENT_3D('',#11712,#9330,#9331);
#7615=AXIS2_PLACEMENT_3D('',#11714,#9332,#9333);
#7616=AXIS2_PLACEMENT_3D('',#11716,#9334,#9335);
#7617=AXIS2_PLACEMENT_3D('',#11717,#9336,#9337);
#7618=AXIS2_PLACEMENT_3D('',#11719,#9338,#9339);
#7619=AXIS2_PLACEMENT_3D('',#11721,#9340,#9341);
#7620=AXIS2_PLACEMENT_3D('',#11722,#9342,#9343);
#7621=AXIS2_PLACEMENT_3D('',#11724,#9345,#9346);
#7622=AXIS2_PLACEMENT_3D('',#11727,#9348,#9349);
#7623=AXIS2_PLACEMENT_3D('',#11728,#9350,#9351);
#7624=AXIS2_PLACEMENT_3D('',#11730,#9352,#9353);
#7625=AXIS2_PLACEMENT_3D('',#11732,#9355,#9356);
#7626=AXIS2_PLACEMENT_3D('',#11733,#9357,#9358);
#7627=AXIS2_PLACEMENT_3D('',#11734,#9359,#9360);
#7628=AXIS2_PLACEMENT_3D('',#11735,#9361,#9362);
#7629=AXIS2_PLACEMENT_3D('',#11737,#9363,#9364);
#7630=AXIS2_PLACEMENT_3D('',#11740,#9366,#9367);
#7631=AXIS2_PLACEMENT_3D('',#11741,#9368,#9369);
#7632=AXIS2_PLACEMENT_3D('',#11743,#9370,#9371);
#7633=AXIS2_PLACEMENT_3D('',#11746,#9373,#9374);
#7634=AXIS2_PLACEMENT_3D('',#11747,#9375,#9376);
#7635=AXIS2_PLACEMENT_3D('',#11748,#9377,#9378);
#7636=AXIS2_PLACEMENT_3D('',#11749,#9379,#9380);
#7637=AXIS2_PLACEMENT_3D('',#11750,#9381,#9382);
#7638=AXIS2_PLACEMENT_3D('',#11752,#9383,#9384);
#7639=AXIS2_PLACEMENT_3D('',#11755,#9386,#9387);
#7640=AXIS2_PLACEMENT_3D('',#11756,#9388,#9389);
#7641=AXIS2_PLACEMENT_3D('',#11758,#9390,#9391);
#7642=AXIS2_PLACEMENT_3D('',#11761,#9393,#9394);
#7643=AXIS2_PLACEMENT_3D('',#11762,#9395,#9396);
#7644=AXIS2_PLACEMENT_3D('',#11763,#9397,#9398);
#7645=AXIS2_PLACEMENT_3D('',#11764,#9399,#9400);
#7646=AXIS2_PLACEMENT_3D('',#11765,#9401,#9402);
#7647=AXIS2_PLACEMENT_3D('',#11767,#9403,#9404);
#7648=AXIS2_PLACEMENT_3D('',#11770,#9406,#9407);
#7649=AXIS2_PLACEMENT_3D('',#11771,#9408,#9409);
#7650=AXIS2_PLACEMENT_3D('',#11773,#9410,#9411);
#7651=AXIS2_PLACEMENT_3D('',#11776,#9413,#9414);
#7652=AXIS2_PLACEMENT_3D('',#11777,#9415,#9416);
#7653=AXIS2_PLACEMENT_3D('',#11778,#9417,#9418);
#7654=AXIS2_PLACEMENT_3D('',#11779,#9419,#9420);
#7655=AXIS2_PLACEMENT_3D('',#11780,#9421,#9422);
#7656=AXIS2_PLACEMENT_3D('',#11782,#9423,#9424);
#7657=AXIS2_PLACEMENT_3D('',#11785,#9426,#9427);
#7658=AXIS2_PLACEMENT_3D('',#11786,#9428,#9429);
#7659=AXIS2_PLACEMENT_3D('',#11788,#9430,#9431);
#7660=AXIS2_PLACEMENT_3D('',#11791,#9433,#9434);
#7661=AXIS2_PLACEMENT_3D('',#11792,#9435,#9436);
#7662=AXIS2_PLACEMENT_3D('',#11793,#9437,#9438);
#7663=AXIS2_PLACEMENT_3D('',#11794,#9439,#9440);
#7664=AXIS2_PLACEMENT_3D('',#11795,#9441,#9442);
#7665=AXIS2_PLACEMENT_3D('',#11797,#9443,#9444);
#7666=AXIS2_PLACEMENT_3D('',#11798,#9445,#9446);
#7667=AXIS2_PLACEMENT_3D('',#11807,#9451,#9452);
#7668=AXIS2_PLACEMENT_3D('',#11813,#9456,#9457);
#7669=AXIS2_PLACEMENT_3D('',#11819,#9461,#9462);
#7670=AXIS2_PLACEMENT_3D('',#11825,#9466,#9467);
#7671=AXIS2_PLACEMENT_3D('',#11831,#9471,#9472);
#7672=AXIS2_PLACEMENT_3D('',#11834,#9475,#9476);
#7673=AXIS2_PLACEMENT_3D('',#11835,#9477,#9478);
#7674=AXIS2_PLACEMENT_3D('',#11837,#9479,#9480);
#7675=AXIS2_PLACEMENT_3D('',#11838,#9481,#9482);
#7676=AXIS2_PLACEMENT_3D('',#11840,#9483,#9484);
#7677=AXIS2_PLACEMENT_3D('',#11842,#9486,#9487);
#7678=AXIS2_PLACEMENT_3D('',#11844,#9489,#9490);
#7679=AXIS2_PLACEMENT_3D('',#11845,#9491,#9492);
#7680=AXIS2_PLACEMENT_3D('',#11854,#9497,#9498);
#7681=AXIS2_PLACEMENT_3D('',#11860,#9502,#9503);
#7682=AXIS2_PLACEMENT_3D('',#11866,#9507,#9508);
#7683=AXIS2_PLACEMENT_3D('',#11872,#9512,#9513);
#7684=AXIS2_PLACEMENT_3D('',#11878,#9517,#9518);
#7685=AXIS2_PLACEMENT_3D('',#11881,#9521,#9522);
#7686=AXIS2_PLACEMENT_3D('',#11882,#9523,#9524);
#7687=AXIS2_PLACEMENT_3D('',#11883,#9525,#9526);
#7688=AXIS2_PLACEMENT_3D('',#11885,#9527,#9528);
#7689=AXIS2_PLACEMENT_3D('',#11886,#9529,#9530);
#7690=AXIS2_PLACEMENT_3D('',#11888,#9531,#9532);
#7691=AXIS2_PLACEMENT_3D('',#11889,#9533,#9534);
#7692=AXIS2_PLACEMENT_3D('',#11891,#9535,#9536);
#7693=AXIS2_PLACEMENT_3D('',#11893,#9538,#9539);
#7694=AXIS2_PLACEMENT_3D('',#11895,#9540,#9541);
#7695=AXIS2_PLACEMENT_3D('',#11897,#9543,#9544);
#7696=AXIS2_PLACEMENT_3D('',#11899,#9545,#9546);
#7697=AXIS2_PLACEMENT_3D('',#11901,#9548,#9549);
#7698=AXIS2_PLACEMENT_3D('',#11903,#9550,#9551);
#7699=AXIS2_PLACEMENT_3D('',#11904,#9552,#9553);
#7700=AXIS2_PLACEMENT_3D('',#11906,#9554,#9555);
#7701=AXIS2_PLACEMENT_3D('',#11908,#9557,#9558);
#7702=AXIS2_PLACEMENT_3D('',#11910,#9560,#9561);
#7703=AXIS2_PLACEMENT_3D('',#11911,#9562,#9563);
#7704=AXIS2_PLACEMENT_3D('',#11913,#9564,#9565);
#7705=AXIS2_PLACEMENT_3D('',#11914,#9566,#9567);
#7706=AXIS2_PLACEMENT_3D('',#11916,#9568,#9569);
#7707=AXIS2_PLACEMENT_3D('',#11918,#9571,#9572);
#7708=AXIS2_PLACEMENT_3D('',#11920,#9573,#9574);
#7709=AXIS2_PLACEMENT_3D('',#11922,#9576,#9577);
#7710=AXIS2_PLACEMENT_3D('',#11924,#9578,#9579);
#7711=AXIS2_PLACEMENT_3D('',#11926,#9581,#9582);
#7712=AXIS2_PLACEMENT_3D('',#11928,#9583,#9584);
#7713=AXIS2_PLACEMENT_3D('',#11929,#9585,#9586);
#7714=AXIS2_PLACEMENT_3D('',#11931,#9587,#9588);
#7715=AXIS2_PLACEMENT_3D('',#11933,#9590,#9591);
#7716=AXIS2_PLACEMENT_3D('',#11935,#9592,#9593);
#7717=AXIS2_PLACEMENT_3D('',#11937,#9595,#9596);
#7718=AXIS2_PLACEMENT_3D('',#11939,#9597,#9598);
#7719=AXIS2_PLACEMENT_3D('',#11941,#9600,#9601);
#7720=AXIS2_PLACEMENT_3D('',#11942,#9602,#9603);
#7721=AXIS2_PLACEMENT_3D('',#11951,#9608,#9609);
#7722=AXIS2_PLACEMENT_3D('',#11957,#9613,#9614);
#7723=AXIS2_PLACEMENT_3D('',#11963,#9618,#9619);
#7724=AXIS2_PLACEMENT_3D('',#11969,#9623,#9624);
#7725=AXIS2_PLACEMENT_3D('',#11975,#9628,#9629);
#7726=AXIS2_PLACEMENT_3D('',#11978,#9632,#9633);
#7727=AXIS2_PLACEMENT_3D('',#11979,#9634,#9635);
#7728=AXIS2_PLACEMENT_3D('',#11980,#9636,#9637);
#7729=AXIS2_PLACEMENT_3D('',#11981,#9638,#9639);
#7730=AXIS2_PLACEMENT_3D('',#11982,#9640,#9641);
#7731=AXIS2_PLACEMENT_3D('',#11983,#9642,#9643);
#7732=AXIS2_PLACEMENT_3D('',#11984,#9644,#9645);
#7733=AXIS2_PLACEMENT_3D('',#11985,#9646,#9647);
#7734=AXIS2_PLACEMENT_3D('',#11986,#9648,#9649);
#7735=AXIS2_PLACEMENT_3D('',#11987,#9650,#9651);
#7736=AXIS2_PLACEMENT_3D('',#11988,#9652,#9653);
#7737=AXIS2_PLACEMENT_3D('',#11989,#9654,#9655);
#7738=AXIS2_PLACEMENT_3D('',#11990,#9656,#9657);
#7739=AXIS2_PLACEMENT_3D('',#11991,#9658,#9659);
#7740=AXIS2_PLACEMENT_3D('',#11992,#9660,#9661);
#7741=AXIS2_PLACEMENT_3D('',#11993,#9662,#9663);
#7742=AXIS2_PLACEMENT_3D('',#11994,#9664,#9665);
#7743=AXIS2_PLACEMENT_3D('',#11995,#9666,#9667);
#7744=AXIS2_PLACEMENT_3D('',#11996,#9668,#9669);
#7745=AXIS2_PLACEMENT_3D('',#11997,#9670,#9671);
#7746=AXIS2_PLACEMENT_3D('',#11998,#9672,#9673);
#7747=AXIS2_PLACEMENT_3D('',#11999,#9674,#9675);
#7748=AXIS2_PLACEMENT_3D('',#12000,#9676,#9677);
#7749=AXIS2_PLACEMENT_3D('',#12001,#9678,#9679);
#7750=AXIS2_PLACEMENT_3D('',#12002,#9680,#9681);
#7751=AXIS2_PLACEMENT_3D('',#12003,#9682,#9683);
#7752=AXIS2_PLACEMENT_3D('',#12004,#9684,#9685);
#7753=AXIS2_PLACEMENT_3D('',#12005,#9686,#9687);
#7754=AXIS2_PLACEMENT_3D('',#12006,#9688,#9689);
#7755=AXIS2_PLACEMENT_3D('',#12007,#9690,#9691);
#7756=AXIS2_PLACEMENT_3D('',#12008,#9692,#9693);
#7757=AXIS2_PLACEMENT_3D('',#12009,#9694,#9695);
#7758=AXIS2_PLACEMENT_3D('',#12010,#9696,#9697);
#7759=AXIS2_PLACEMENT_3D('',#12011,#9698,#9699);
#7760=AXIS2_PLACEMENT_3D('',#12012,#9700,#9701);
#7761=AXIS2_PLACEMENT_3D('',#12013,#9702,#9703);
#7762=AXIS2_PLACEMENT_3D('',#12014,#9704,#9705);
#7763=AXIS2_PLACEMENT_3D('',#12015,#9706,#9707);
#7764=AXIS2_PLACEMENT_3D('',#12016,#9708,#9709);
#7765=AXIS2_PLACEMENT_3D('',#12017,#9710,#9711);
#7766=AXIS2_PLACEMENT_3D('',#12018,#9712,#9713);
#7767=AXIS2_PLACEMENT_3D('',#12019,#9714,#9715);
#7768=AXIS2_PLACEMENT_3D('',#12020,#9716,#9717);
#7769=AXIS2_PLACEMENT_3D('',#12021,#9718,#9719);
#7770=AXIS2_PLACEMENT_3D('',#12022,#9720,#9721);
#7771=AXIS2_PLACEMENT_3D('',#12023,#9722,#9723);
#7772=AXIS2_PLACEMENT_3D('',#12024,#9724,#9725);
#7773=AXIS2_PLACEMENT_3D('',#12025,#9726,#9727);
#7774=AXIS2_PLACEMENT_3D('',#12026,#9728,#9729);
#7775=AXIS2_PLACEMENT_3D('',#12027,#9730,#9731);
#7776=AXIS2_PLACEMENT_3D('',#12029,#9732,#9733);
#7777=AXIS2_PLACEMENT_3D('',#12032,#9735,#9736);
#7778=AXIS2_PLACEMENT_3D('',#12033,#9737,#9738);
#7779=AXIS2_PLACEMENT_3D('',#12035,#9739,#9740);
#7780=AXIS2_PLACEMENT_3D('',#12038,#9742,#9743);
#7781=AXIS2_PLACEMENT_3D('',#12039,#9744,#9745);
#7782=AXIS2_PLACEMENT_3D('',#12044,#9747,#9748);
#7783=AXIS2_PLACEMENT_3D('',#12047,#9750,#9751);
#7784=AXIS2_PLACEMENT_3D('',#12048,#9752,#9753);
#7785=AXIS2_PLACEMENT_3D('',#12054,#9757,#9758);
#7786=AXIS2_PLACEMENT_3D('',#12057,#9760,#9761);
#7787=AXIS2_PLACEMENT_3D('',#12058,#9762,#9763);
#7788=AXIS2_PLACEMENT_3D('',#12062,#9766,#9767);
#7789=AXIS2_PLACEMENT_3D('',#12063,#9768,#9769);
#7790=AXIS2_PLACEMENT_3D('',#12064,#9770,#9771);
#7791=AXIS2_PLACEMENT_3D('',#12065,#9772,#9773);
#7792=AXIS2_PLACEMENT_3D('',#12066,#9774,#9775);
#7793=AXIS2_PLACEMENT_3D('',#12068,#9776,#9777);
#7794=AXIS2_PLACEMENT_3D('',#12071,#9779,#9780);
#7795=AXIS2_PLACEMENT_3D('',#12072,#9781,#9782);
#7796=AXIS2_PLACEMENT_3D('',#12074,#9783,#9784);
#7797=AXIS2_PLACEMENT_3D('',#12077,#9786,#9787);
#7798=AXIS2_PLACEMENT_3D('',#12078,#9788,#9789);
#7799=AXIS2_PLACEMENT_3D('',#12079,#9790,#9791);
#7800=AXIS2_PLACEMENT_3D('',#12080,#9792,#9793);
#7801=AXIS2_PLACEMENT_3D('',#12081,#9794,#9795);
#7802=AXIS2_PLACEMENT_3D('',#12083,#9796,#9797);
#7803=AXIS2_PLACEMENT_3D('',#12086,#9799,#9800);
#7804=AXIS2_PLACEMENT_3D('',#12087,#9801,#9802);
#7805=AXIS2_PLACEMENT_3D('',#12089,#9803,#9804);
#7806=AXIS2_PLACEMENT_3D('',#12092,#9806,#9807);
#7807=AXIS2_PLACEMENT_3D('',#12093,#9808,#9809);
#7808=AXIS2_PLACEMENT_3D('',#12094,#9810,#9811);
#7809=AXIS2_PLACEMENT_3D('',#12095,#9812,#9813);
#7810=AXIS2_PLACEMENT_3D('',#12096,#9814,#9815);
#7811=AXIS2_PLACEMENT_3D('',#12097,#9816,#9817);
#7812=AXIS2_PLACEMENT_3D('',#12098,#9818,#9819);
#7813=AXIS2_PLACEMENT_3D('',#12099,#9820,#9821);
#7814=AXIS2_PLACEMENT_3D('',#12100,#9822,#9823);
#7815=AXIS2_PLACEMENT_3D('',#12102,#9824,#9825);
#7816=AXIS2_PLACEMENT_3D('',#12105,#9827,#9828);
#7817=AXIS2_PLACEMENT_3D('',#12106,#9829,#9830);
#7818=AXIS2_PLACEMENT_3D('',#12107,#9831,#9832);
#7819=AXIS2_PLACEMENT_3D('',#12116,#9837,#9838);
#7820=AXIS2_PLACEMENT_3D('',#12126,#9844,#9845);
#7821=AXIS2_PLACEMENT_3D('',#12129,#9847,#9848);
#7822=AXIS2_PLACEMENT_3D('',#12130,#9849,#9850);
#7823=AXIS2_PLACEMENT_3D('',#12138,#9855,#9856);
#7824=AXIS2_PLACEMENT_3D('',#12144,#9860,#9861);
#7825=AXIS2_PLACEMENT_3D('',#12150,#9865,#9866);
#7826=AXIS2_PLACEMENT_3D('',#12151,#9867,#9868);
#7827=AXIS2_PLACEMENT_3D('',#12152,#9869,#9870);
#7828=AXIS2_PLACEMENT_3D('',#12154,#9871,#9872);
#7829=AXIS2_PLACEMENT_3D('',#12156,#9874,#9875);
#7830=AXIS2_PLACEMENT_3D('',#12157,#9876,#9877);
#7831=AXIS2_PLACEMENT_3D('',#12159,#9878,#9879);
#7832=AXIS2_PLACEMENT_3D('',#12160,#9880,#9881);
#7833=AXIS2_PLACEMENT_3D('',#12161,#9882,#9883);
#7834=AXIS2_PLACEMENT_3D('',#12164,#9885,#9886);
#7835=AXIS2_PLACEMENT_3D('',#12165,#9887,#9888);
#7836=AXIS2_PLACEMENT_3D('',#12166,#9889,#9890);
#7837=AXIS2_PLACEMENT_3D('',#12167,#9891,#9892);
#7838=AXIS2_PLACEMENT_3D('',#12171,#9894,#9895);
#7839=AXIS2_PLACEMENT_3D('',#12172,#9896,#9897);
#7840=AXIS2_PLACEMENT_3D('',#12185,#9898,#9899);
#7841=AXIS2_PLACEMENT_3D('',#12188,#9901,#9902);
#7842=AXIS2_PLACEMENT_3D('',#12190,#9903,#9904);
#7843=AXIS2_PLACEMENT_3D('',#12201,#9905,#9906);
#7844=AXIS2_PLACEMENT_3D('',#12203,#9908,#9909);
#7845=AXIS2_PLACEMENT_3D('',#12205,#9910,#9911);
#7846=AXIS2_PLACEMENT_3D('',#12208,#9913,#9914);
#7847=AXIS2_PLACEMENT_3D('',#12209,#9915,#9916);
#7848=AXIS2_PLACEMENT_3D('',#12218,#9921,#9922);
#7849=AXIS2_PLACEMENT_3D('',#12224,#9926,#9927);
#7850=AXIS2_PLACEMENT_3D('',#12228,#9930,#9931);
#7851=AXIS2_PLACEMENT_3D('',#12232,#9934,#9935);
#7852=AXIS2_PLACEMENT_3D('',#12234,#9937,#9938);
#7853=AXIS2_PLACEMENT_3D('',#12235,#9939,#9940);
#7854=AXIS2_PLACEMENT_3D('',#12236,#9941,#9942);
#7855=AXIS2_PLACEMENT_3D('',#12238,#9943,#9944);
#7856=AXIS2_PLACEMENT_3D('',#12240,#9945,#9946);
#7857=AXIS2_PLACEMENT_3D('',#12241,#9947,#9948);
#7858=AXIS2_PLACEMENT_3D('',#12244,#9950,#9951);
#7859=AXIS2_PLACEMENT_3D('',#12245,#9952,#9953);
#7860=AXIS2_PLACEMENT_3D('',#12246,#9954,#9955);
#7861=AXIS2_PLACEMENT_3D('',#12248,#9956,#9957);
#7862=AXIS2_PLACEMENT_3D('',#12250,#9959,#9960);
#7863=AXIS2_PLACEMENT_3D('',#12251,#9961,#9962);
#7864=AXIS2_PLACEMENT_3D('',#12252,#9963,#9964);
#7865=AXIS2_PLACEMENT_3D('',#12254,#9965,#9966);
#7866=AXIS2_PLACEMENT_3D('',#12257,#9968,#9969);
#7867=AXIS2_PLACEMENT_3D('',#12258,#9970,#9971);
#7868=AXIS2_PLACEMENT_3D('',#12259,#9972,#9973);
#7869=AXIS2_PLACEMENT_3D('',#12260,#9974,#9975);
#7870=AXIS2_PLACEMENT_3D('',#12261,#9976,#9977);
#7871=AXIS2_PLACEMENT_3D('',#12270,#9982,#9983);
#7872=AXIS2_PLACEMENT_3D('',#12276,#9987,#9988);
#7873=AXIS2_PLACEMENT_3D('',#12282,#9992,#9993);
#7874=AXIS2_PLACEMENT_3D('',#12288,#9997,#9998);
#7875=AXIS2_PLACEMENT_3D('',#12294,#10002,#10003);
#7876=AXIS2_PLACEMENT_3D('',#12297,#10006,#10007);
#7877=AXIS2_PLACEMENT_3D('',#12298,#10008,#10009);
#7878=AXIS2_PLACEMENT_3D('',#12300,#10010,#10011);
#7879=AXIS2_PLACEMENT_3D('',#12301,#10012,#10013);
#7880=AXIS2_PLACEMENT_3D('',#12303,#10014,#10015);
#7881=AXIS2_PLACEMENT_3D('',#12305,#10017,#10018);
#7882=AXIS2_PLACEMENT_3D('',#12307,#10019,#10020);
#7883=AXIS2_PLACEMENT_3D('',#12309,#10022,#10023);
#7884=AXIS2_PLACEMENT_3D('',#12311,#10024,#10025);
#7885=AXIS2_PLACEMENT_3D('',#12313,#10027,#10028);
#7886=AXIS2_PLACEMENT_3D('',#12314,#10029,#10030);
#7887=AXIS2_PLACEMENT_3D('',#12315,#10031,#10032);
#7888=AXIS2_PLACEMENT_3D('',#12316,#10033,#10034);
#7889=AXIS2_PLACEMENT_3D('',#12317,#10035,#10036);
#7890=AXIS2_PLACEMENT_3D('',#12318,#10037,#10038);
#7891=AXIS2_PLACEMENT_3D('',#12319,#10039,#10040);
#7892=AXIS2_PLACEMENT_3D('',#12320,#10041,#10042);
#7893=AXIS2_PLACEMENT_3D('',#12321,#10043,#10044);
#7894=DIRECTION('axis',(0.,0.,1.));
#7895=DIRECTION('refdir',(1.,0.,0.));
#7896=DIRECTION('axis',(0.,0.,1.));
#7897=DIRECTION('refdir',(1.,0.,0.));
#7898=DIRECTION('axis',(0.,0.,1.));
#7899=DIRECTION('refdir',(1.,0.,0.));
#7900=DIRECTION('center_axis',(0.,0.,1.));
#7901=DIRECTION('ref_axis',(1.,0.,0.));
#7902=DIRECTION('center_axis',(0.,0.,1.));
#7903=DIRECTION('ref_axis',(1.,0.,0.));
#7904=DIRECTION('',(0.,0.,1.));
#7905=DIRECTION('center_axis',(0.,0.,-1.));
#7906=DIRECTION('ref_axis',(1.,0.,0.));
#7907=DIRECTION('center_axis',(0.,0.,1.));
#7908=DIRECTION('ref_axis',(1.,0.,0.));
#7909=DIRECTION('center_axis',(0.,0.,1.));
#7910=DIRECTION('ref_axis',(1.,0.,0.));
#7911=DIRECTION('',(0.,0.,1.));
#7912=DIRECTION('center_axis',(0.,0.,-1.));
#7913=DIRECTION('ref_axis',(1.,0.,0.));
#7914=DIRECTION('center_axis',(0.,0.,1.));
#7915=DIRECTION('ref_axis',(1.,0.,0.));
#7916=DIRECTION('center_axis',(0.,0.,1.));
#7917=DIRECTION('ref_axis',(1.,0.,0.));
#7918=DIRECTION('',(0.,0.,1.));
#7919=DIRECTION('center_axis',(0.,0.,-1.));
#7920=DIRECTION('ref_axis',(1.,0.,0.));
#7921=DIRECTION('center_axis',(0.,0.,1.));
#7922=DIRECTION('ref_axis',(1.,0.,0.));
#7923=DIRECTION('center_axis',(0.,0.,1.));
#7924=DIRECTION('ref_axis',(1.,0.,0.));
#7925=DIRECTION('',(0.,0.,1.));
#7926=DIRECTION('center_axis',(0.,0.,-1.));
#7927=DIRECTION('ref_axis',(1.,0.,0.));
#7928=DIRECTION('center_axis',(0.,0.,1.));
#7929=DIRECTION('ref_axis',(1.,0.,0.));
#7930=DIRECTION('center_axis',(0.,0.,1.));
#7931=DIRECTION('ref_axis',(1.,0.,0.));
#7932=DIRECTION('',(0.,0.,1.));
#7933=DIRECTION('center_axis',(0.,0.,-1.));
#7934=DIRECTION('ref_axis',(1.,0.,0.));
#7935=DIRECTION('center_axis',(0.,0.,1.));
#7936=DIRECTION('ref_axis',(1.,0.,0.));
#7937=DIRECTION('center_axis',(0.,0.,1.));
#7938=DIRECTION('ref_axis',(1.,0.,0.));
#7939=DIRECTION('',(0.,0.,1.));
#7940=DIRECTION('center_axis',(0.,0.,-1.));
#7941=DIRECTION('ref_axis',(1.,0.,0.));
#7942=DIRECTION('center_axis',(0.,0.,1.));
#7943=DIRECTION('ref_axis',(1.,0.,0.));
#7944=DIRECTION('center_axis',(0.,0.,1.));
#7945=DIRECTION('ref_axis',(1.,0.,0.));
#7946=DIRECTION('',(0.,0.,1.));
#7947=DIRECTION('center_axis',(0.,0.,-1.));
#7948=DIRECTION('ref_axis',(1.,0.,0.));
#7949=DIRECTION('center_axis',(0.,0.,1.));
#7950=DIRECTION('ref_axis',(1.,0.,0.));
#7951=DIRECTION('center_axis',(0.,0.,1.));
#7952=DIRECTION('ref_axis',(1.,0.,0.));
#7953=DIRECTION('',(0.,0.,1.));
#7954=DIRECTION('center_axis',(0.,0.,-1.));
#7955=DIRECTION('ref_axis',(1.,0.,0.));
#7956=DIRECTION('center_axis',(0.,1.,0.));
#7957=DIRECTION('ref_axis',(-1.,0.,0.));
#7958=DIRECTION('',(-1.,0.,0.));
#7959=DIRECTION('',(0.,0.,1.));
#7960=DIRECTION('',(-1.,0.,0.));
#7961=DIRECTION('',(0.,0.,1.));
#7962=DIRECTION('center_axis',(1.,0.,0.));
#7963=DIRECTION('ref_axis',(0.,1.,0.));
#7964=DIRECTION('',(0.,1.,0.));
#7965=DIRECTION('',(0.,1.,0.));
#7966=DIRECTION('',(0.,0.,1.));
#7967=DIRECTION('center_axis',(0.,-1.,0.));
#7968=DIRECTION('ref_axis',(1.,0.,0.));
#7969=DIRECTION('',(1.,0.,0.));
#7970=DIRECTION('',(1.,0.,0.));
#7971=DIRECTION('',(0.,0.,1.));
#7972=DIRECTION('center_axis',(-1.,0.,0.));
#7973=DIRECTION('ref_axis',(0.,-1.,0.));
#7974=DIRECTION('',(0.,-1.,0.));
#7975=DIRECTION('',(0.,-1.,0.));
#7976=DIRECTION('center_axis',(0.,0.,1.));
#7977=DIRECTION('ref_axis',(1.,0.,0.));
#7978=DIRECTION('center_axis',(0.,0.,1.));
#7979=DIRECTION('ref_axis',(1.,0.,0.));
#7980=DIRECTION('axis',(0.,0.,1.));
#7981=DIRECTION('refdir',(1.,0.,0.));
#7982=DIRECTION('center_axis',(0.,1.,0.));
#7983=DIRECTION('ref_axis',(-1.,0.,0.));
#7984=DIRECTION('',(-1.,0.,0.));
#7985=DIRECTION('',(0.,0.,1.));
#7986=DIRECTION('',(-1.,0.,0.));
#7987=DIRECTION('',(0.,0.,1.));
#7988=DIRECTION('center_axis',(1.,0.,0.));
#7989=DIRECTION('ref_axis',(0.,1.,0.));
#7990=DIRECTION('',(0.,1.,0.));
#7991=DIRECTION('',(0.,1.,0.));
#7992=DIRECTION('',(0.,0.,1.));
#7993=DIRECTION('center_axis',(0.,-1.,0.));
#7994=DIRECTION('ref_axis',(1.,0.,0.));
#7995=DIRECTION('',(1.,0.,0.));
#7996=DIRECTION('',(1.,0.,0.));
#7997=DIRECTION('',(0.,0.,1.));
#7998=DIRECTION('center_axis',(-1.,0.,0.));
#7999=DIRECTION('ref_axis',(0.,-1.,0.));
#8000=DIRECTION('',(0.,-1.,0.));
#8001=DIRECTION('',(0.,-1.,0.));
#8002=DIRECTION('center_axis',(0.,0.,1.));
#8003=DIRECTION('ref_axis',(1.,0.,0.));
#8004=DIRECTION('center_axis',(0.,0.,1.));
#8005=DIRECTION('ref_axis',(1.,0.,0.));
#8006=DIRECTION('axis',(0.,0.,1.));
#8007=DIRECTION('refdir',(1.,0.,0.));
#8008=DIRECTION('center_axis',(0.,1.,0.));
#8009=DIRECTION('ref_axis',(-1.,0.,0.));
#8010=DIRECTION('',(-1.,0.,0.));
#8011=DIRECTION('',(0.,0.,1.));
#8012=DIRECTION('',(-1.,0.,0.));
#8013=DIRECTION('',(0.,0.,1.));
#8014=DIRECTION('center_axis',(1.,0.,0.));
#8015=DIRECTION('ref_axis',(0.,1.,0.));
#8016=DIRECTION('',(0.,1.,0.));
#8017=DIRECTION('',(0.,1.,0.));
#8018=DIRECTION('',(0.,0.,1.));
#8019=DIRECTION('center_axis',(0.,-1.,0.));
#8020=DIRECTION('ref_axis',(1.,0.,0.));
#8021=DIRECTION('',(1.,0.,0.));
#8022=DIRECTION('',(1.,0.,0.));
#8023=DIRECTION('',(0.,0.,1.));
#8024=DIRECTION('center_axis',(-1.,0.,0.));
#8025=DIRECTION('ref_axis',(0.,-1.,0.));
#8026=DIRECTION('',(0.,-1.,0.));
#8027=DIRECTION('',(0.,-1.,0.));
#8028=DIRECTION('center_axis',(0.,0.,1.));
#8029=DIRECTION('ref_axis',(1.,0.,0.));
#8030=DIRECTION('center_axis',(0.,0.,1.));
#8031=DIRECTION('ref_axis',(1.,0.,0.));
#8032=DIRECTION('axis',(0.,0.,1.));
#8033=DIRECTION('refdir',(1.,0.,0.));
#8034=DIRECTION('center_axis',(0.,1.,0.));
#8035=DIRECTION('ref_axis',(1.,0.,0.));
#8036=DIRECTION('center_axis',(0.,1.,0.));
#8037=DIRECTION('ref_axis',(1.,0.,0.));
#8038=DIRECTION('',(0.,1.,0.));
#8039=DIRECTION('center_axis',(0.,-1.,0.));
#8040=DIRECTION('ref_axis',(1.,0.,0.));
#8041=DIRECTION('center_axis',(0.,0.,1.));
#8042=DIRECTION('ref_axis',(1.,0.,0.));
#8043=DIRECTION('center_axis',(0.,0.,1.));
#8044=DIRECTION('ref_axis',(1.,0.,0.));
#8045=DIRECTION('',(0.,0.,1.));
#8046=DIRECTION('center_axis',(0.,0.,-1.));
#8047=DIRECTION('ref_axis',(1.,0.,0.));
#8048=DIRECTION('center_axis',(0.,0.,1.));
#8049=DIRECTION('ref_axis',(1.,0.,0.));
#8050=DIRECTION('center_axis',(0.,0.,1.));
#8051=DIRECTION('ref_axis',(1.,0.,0.));
#8052=DIRECTION('center_axis',(0.,0.,1.));
#8053=DIRECTION('ref_axis',(1.,0.,0.));
#8054=DIRECTION('',(0.,0.,1.));
#8055=DIRECTION('center_axis',(0.,0.,-1.));
#8056=DIRECTION('ref_axis',(1.,0.,0.));
#8057=DIRECTION('center_axis',(0.,0.,1.));
#8058=DIRECTION('ref_axis',(1.,0.,0.));
#8059=DIRECTION('center_axis',(0.,0.,1.));
#8060=DIRECTION('ref_axis',(1.,0.,0.));
#8061=DIRECTION('center_axis',(0.,0.,1.));
#8062=DIRECTION('ref_axis',(1.,0.,0.));
#8063=DIRECTION('',(0.,0.,1.));
#8064=DIRECTION('center_axis',(0.,0.,-1.));
#8065=DIRECTION('ref_axis',(1.,0.,0.));
#8066=DIRECTION('center_axis',(0.,0.,1.));
#8067=DIRECTION('ref_axis',(1.,0.,0.));
#8068=DIRECTION('center_axis',(0.,0.,1.));
#8069=DIRECTION('ref_axis',(1.,0.,0.));
#8070=DIRECTION('center_axis',(0.,0.,1.));
#8071=DIRECTION('ref_axis',(1.,0.,0.));
#8072=DIRECTION('',(0.,0.,1.));
#8073=DIRECTION('center_axis',(0.,0.,-1.));
#8074=DIRECTION('ref_axis',(1.,0.,0.));
#8075=DIRECTION('center_axis',(0.,0.,1.));
#8076=DIRECTION('ref_axis',(1.,0.,0.));
#8077=DIRECTION('center_axis',(0.,1.,0.));
#8078=DIRECTION('ref_axis',(1.,0.,0.));
#8079=DIRECTION('center_axis',(0.,1.,0.));
#8080=DIRECTION('ref_axis',(1.,0.,0.));
#8081=DIRECTION('',(0.,1.,0.));
#8082=DIRECTION('center_axis',(0.,-1.,0.));
#8083=DIRECTION('ref_axis',(1.,0.,0.));
#8084=DIRECTION('center_axis',(0.,1.,0.));
#8085=DIRECTION('ref_axis',(1.,0.,0.));
#8086=DIRECTION('center_axis',(0.,1.,0.));
#8087=DIRECTION('ref_axis',(1.,0.,0.));
#8088=DIRECTION('',(0.,1.,0.));
#8089=DIRECTION('center_axis',(0.,-1.,0.));
#8090=DIRECTION('ref_axis',(1.,0.,0.));
#8091=DIRECTION('center_axis',(0.,1.,0.));
#8092=DIRECTION('ref_axis',(1.,0.,0.));
#8093=DIRECTION('center_axis',(0.,1.,0.));
#8094=DIRECTION('ref_axis',(1.,0.,0.));
#8095=DIRECTION('',(0.,1.,0.));
#8096=DIRECTION('center_axis',(0.,-1.,0.));
#8097=DIRECTION('ref_axis',(1.,0.,0.));
#8098=DIRECTION('center_axis',(0.,1.,0.));
#8099=DIRECTION('ref_axis',(1.,0.,0.));
#8100=DIRECTION('center_axis',(0.,1.,0.));
#8101=DIRECTION('ref_axis',(1.,0.,0.));
#8102=DIRECTION('',(0.,1.,0.));
#8103=DIRECTION('center_axis',(0.,-1.,0.));
#8104=DIRECTION('ref_axis',(1.,0.,0.));
#8105=DIRECTION('center_axis',(0.,0.,1.));
#8106=DIRECTION('ref_axis',(1.,0.,0.));
#8107=DIRECTION('center_axis',(0.,0.,1.));
#8108=DIRECTION('ref_axis',(1.,0.,0.));
#8109=DIRECTION('',(0.,0.,1.));
#8110=DIRECTION('center_axis',(0.,0.,-1.));
#8111=DIRECTION('ref_axis',(1.,0.,0.));
#8112=DIRECTION('center_axis',(0.,0.,1.));
#8113=DIRECTION('ref_axis',(1.,0.,0.));
#8114=DIRECTION('center_axis',(0.,0.,1.));
#8115=DIRECTION('ref_axis',(1.,0.,0.));
#8116=DIRECTION('',(0.,0.,1.));
#8117=DIRECTION('center_axis',(0.,0.,-1.));
#8118=DIRECTION('ref_axis',(1.,0.,0.));
#8119=DIRECTION('center_axis',(0.,0.,1.));
#8120=DIRECTION('ref_axis',(1.,0.,0.));
#8121=DIRECTION('center_axis',(0.,0.,1.));
#8122=DIRECTION('ref_axis',(1.,0.,0.));
#8123=DIRECTION('',(0.,0.,1.));
#8124=DIRECTION('center_axis',(0.,0.,-1.));
#8125=DIRECTION('ref_axis',(1.,0.,0.));
#8126=DIRECTION('center_axis',(0.,0.,1.));
#8127=DIRECTION('ref_axis',(1.,0.,0.));
#8128=DIRECTION('center_axis',(0.,0.,1.));
#8129=DIRECTION('ref_axis',(1.,0.,0.));
#8130=DIRECTION('',(0.,0.,1.));
#8131=DIRECTION('center_axis',(0.,0.,-1.));
#8132=DIRECTION('ref_axis',(1.,0.,0.));
#8133=DIRECTION('center_axis',(0.,0.,1.));
#8134=DIRECTION('ref_axis',(1.,0.,0.));
#8135=DIRECTION('center_axis',(0.,0.,1.));
#8136=DIRECTION('ref_axis',(1.,0.,0.));
#8137=DIRECTION('',(0.,0.,1.));
#8138=DIRECTION('center_axis',(0.,0.,-1.));
#8139=DIRECTION('ref_axis',(1.,0.,0.));
#8140=DIRECTION('center_axis',(0.,0.,1.));
#8141=DIRECTION('ref_axis',(1.,0.,0.));
#8142=DIRECTION('center_axis',(0.,0.,1.));
#8143=DIRECTION('ref_axis',(1.,0.,0.));
#8144=DIRECTION('center_axis',(0.,0.,1.));
#8145=DIRECTION('ref_axis',(1.,0.,0.));
#8146=DIRECTION('center_axis',(0.,0.,1.));
#8147=DIRECTION('ref_axis',(1.,0.,0.));
#8148=DIRECTION('',(0.,0.,1.));
#8149=DIRECTION('center_axis',(0.,1.,0.));
#8150=DIRECTION('ref_axis',(1.,0.,0.));
#8151=DIRECTION('center_axis',(0.,1.,0.));
#8152=DIRECTION('ref_axis',(1.,0.,0.));
#8153=DIRECTION('',(0.,1.,0.));
#8154=DIRECTION('center_axis',(0.,-1.,0.));
#8155=DIRECTION('ref_axis',(1.,0.,0.));
#8156=DIRECTION('center_axis',(0.,0.,1.));
#8157=DIRECTION('ref_axis',(1.,0.,0.));
#8158=DIRECTION('',(0.,0.,1.));
#8159=DIRECTION('center_axis',(0.,0.,1.));
#8160=DIRECTION('ref_axis',(1.,0.,0.));
#8161=DIRECTION('',(0.,0.,-1.));
#8162=DIRECTION('center_axis',(0.,0.,1.));
#8163=DIRECTION('ref_axis',(1.,0.,0.));
#8164=DIRECTION('center_axis',(0.,-1.,0.));
#8165=DIRECTION('ref_axis',(1.,0.,0.));
#8166=DIRECTION('',(-1.,0.,0.));
#8167=DIRECTION('',(0.,0.,1.));
#8168=DIRECTION('',(1.,0.,0.));
#8169=DIRECTION('',(0.,0.,1.));
#8170=DIRECTION('',(1.,0.,0.));
#8171=DIRECTION('',(0.,0.,1.));
#8172=DIRECTION('',(1.,0.,0.));
#8173=DIRECTION('center_axis',(0.,1.,0.));
#8174=DIRECTION('ref_axis',(1.,0.,0.));
#8175=DIRECTION('',(1.,0.,0.));
#8176=DIRECTION('center_axis',(0.,0.,1.));
#8177=DIRECTION('ref_axis',(1.,0.,0.));
#8178=DIRECTION('',(1.,0.,0.));
#8179=DIRECTION('',(0.,1.,0.));
#8180=DIRECTION('center_axis',(0.,0.,1.));
#8181=DIRECTION('ref_axis',(1.,0.,0.));
#8182=DIRECTION('',(0.,-1.,0.));
#8183=DIRECTION('',(1.,0.,0.));
#8184=DIRECTION('',(0.,1.,0.));
#8185=DIRECTION('',(-1.,0.,0.));
#8186=DIRECTION('',(-1.,0.,0.));
#8187=DIRECTION('',(0.,1.,0.));
#8188=DIRECTION('',(0.,-1.,0.));
#8189=DIRECTION('center_axis',(0.,1.,0.));
#8190=DIRECTION('ref_axis',(-1.,0.,0.));
#8191=DIRECTION('',(-1.,0.,0.));
#8192=DIRECTION('',(0.,0.,1.));
#8193=DIRECTION('',(0.,0.,1.));
#8194=DIRECTION('center_axis',(1.,0.,0.));
#8195=DIRECTION('ref_axis',(0.,1.,0.));
#8196=DIRECTION('',(0.,1.,0.));
#8197=DIRECTION('',(0.,0.,1.));
#8198=DIRECTION('center_axis',(0.,-1.,0.));
#8199=DIRECTION('ref_axis',(1.,0.,0.));
#8200=DIRECTION('',(1.,0.,0.));
#8201=DIRECTION('',(0.,0.,1.));
#8202=DIRECTION('center_axis',(-1.,0.,0.));
#8203=DIRECTION('ref_axis',(0.,-1.,0.));
#8204=DIRECTION('',(0.,-1.,0.));
#8205=DIRECTION('center_axis',(1.,0.,0.));
#8206=DIRECTION('ref_axis',(0.,1.,0.));
#8207=DIRECTION('',(0.,0.,1.));
#8208=DIRECTION('',(0.,-1.,0.));
#8209=DIRECTION('center_axis',(0.,1.,0.));
#8210=DIRECTION('ref_axis',(6.12323399573677E-17,0.,-1.));
#8211=DIRECTION('',(0.,1.,0.));
#8212=DIRECTION('',(0.,-1.,0.));
#8213=DIRECTION('center_axis',(0.,1.,0.));
#8214=DIRECTION('ref_axis',(1.,0.,0.));
#8215=DIRECTION('center_axis',(0.,1.,0.));
#8216=DIRECTION('ref_axis',(-1.,0.,0.));
#8217=DIRECTION('',(-1.,0.,0.));
#8218=DIRECTION('',(-1.,0.,0.));
#8219=DIRECTION('',(0.,0.,1.));
#8220=DIRECTION('',(-1.,0.,0.));
#8221=DIRECTION('',(0.,0.,1.));
#8222=DIRECTION('center_axis',(0.,0.,-1.));
#8223=DIRECTION('ref_axis',(-1.,0.,0.));
#8224=DIRECTION('center_axis',(0.,0.,-1.));
#8225=DIRECTION('ref_axis',(-1.,0.,0.));
#8226=DIRECTION('center_axis',(1.,0.,0.));
#8227=DIRECTION('ref_axis',(0.,1.,0.));
#8228=DIRECTION('',(0.,1.,0.));
#8229=DIRECTION('center_axis',(-1.,0.,0.));
#8230=DIRECTION('ref_axis',(0.,-1.,0.));
#8231=DIRECTION('',(0.,-1.,0.));
#8232=DIRECTION('center_axis',(0.,0.,1.));
#8233=DIRECTION('ref_axis',(1.,0.,0.));
#8234=DIRECTION('center_axis',(0.,0.,1.));
#8235=DIRECTION('ref_axis',(1.,0.,0.));
#8236=DIRECTION('axis',(0.,0.,1.));
#8237=DIRECTION('refdir',(1.,0.,0.));
#8238=DIRECTION('center_axis',(0.,1.,0.));
#8239=DIRECTION('ref_axis',(1.,0.,0.));
#8240=DIRECTION('center_axis',(0.,1.,0.));
#8241=DIRECTION('ref_axis',(1.,0.,0.));
#8242=DIRECTION('',(0.,1.,0.));
#8243=DIRECTION('center_axis',(0.,-1.,0.));
#8244=DIRECTION('ref_axis',(1.,0.,0.));
#8245=DIRECTION('center_axis',(0.,1.,0.));
#8246=DIRECTION('ref_axis',(1.,0.,0.));
#8247=DIRECTION('center_axis',(0.,1.,0.));
#8248=DIRECTION('ref_axis',(1.,0.,0.));
#8249=DIRECTION('',(0.,1.,0.));
#8250=DIRECTION('center_axis',(0.,-1.,0.));
#8251=DIRECTION('ref_axis',(1.,0.,0.));
#8252=DIRECTION('center_axis',(0.,1.,0.));
#8253=DIRECTION('ref_axis',(1.,0.,0.));
#8254=DIRECTION('center_axis',(0.,1.,0.));
#8255=DIRECTION('ref_axis',(1.,0.,0.));
#8256=DIRECTION('',(0.,1.,0.));
#8257=DIRECTION('center_axis',(0.,-1.,0.));
#8258=DIRECTION('ref_axis',(1.,0.,0.));
#8259=DIRECTION('center_axis',(0.,1.,0.));
#8260=DIRECTION('ref_axis',(1.,0.,0.));
#8261=DIRECTION('center_axis',(0.,1.,0.));
#8262=DIRECTION('ref_axis',(1.,0.,0.));
#8263=DIRECTION('',(0.,1.,0.));
#8264=DIRECTION('center_axis',(0.,-1.,0.));
#8265=DIRECTION('ref_axis',(1.,0.,0.));
#8266=DIRECTION('center_axis',(0.,1.,0.));
#8267=DIRECTION('ref_axis',(1.,0.,0.));
#8268=DIRECTION('center_axis',(0.,1.,0.));
#8269=DIRECTION('ref_axis',(1.,0.,0.));
#8270=DIRECTION('',(0.,-1.,0.));
#8271=DIRECTION('center_axis',(0.,-1.,0.));
#8272=DIRECTION('ref_axis',(1.,0.,0.));
#8273=DIRECTION('center_axis',(0.,1.,0.));
#8274=DIRECTION('ref_axis',(1.,0.,0.));
#8275=DIRECTION('center_axis',(0.,-1.,0.));
#8276=DIRECTION('ref_axis',(1.,0.,0.));
#8277=DIRECTION('center_axis',(0.,1.,0.));
#8278=DIRECTION('ref_axis',(1.,0.,0.));
#8279=DIRECTION('',(0.,-1.,0.));
#8280=DIRECTION('center_axis',(0.,-1.,0.));
#8281=DIRECTION('ref_axis',(1.,0.,0.));
#8282=DIRECTION('center_axis',(0.,1.,0.));
#8283=DIRECTION('ref_axis',(1.,0.,0.));
#8284=DIRECTION('center_axis',(0.,1.,0.));
#8285=DIRECTION('ref_axis',(1.,0.,0.));
#8286=DIRECTION('',(0.,-1.,0.));
#8287=DIRECTION('center_axis',(0.,1.,0.));
#8288=DIRECTION('ref_axis',(1.,0.,0.));
#8289=DIRECTION('center_axis',(0.,1.,0.));
#8290=DIRECTION('ref_axis',(1.,0.,0.));
#8291=DIRECTION('center_axis',(0.,1.,0.));
#8292=DIRECTION('ref_axis',(1.,0.,0.));
#8293=DIRECTION('axis',(0.,0.,1.));
#8294=DIRECTION('refdir',(1.,0.,0.));
#8295=DIRECTION('center_axis',(0.,1.,0.));
#8296=DIRECTION('ref_axis',(1.,0.,0.));
#8297=DIRECTION('center_axis',(0.,1.,0.));
#8298=DIRECTION('ref_axis',(1.,0.,0.));
#8299=DIRECTION('',(0.,1.,0.));
#8300=DIRECTION('center_axis',(0.,-1.,0.));
#8301=DIRECTION('ref_axis',(1.,0.,0.));
#8302=DIRECTION('center_axis',(0.,1.,0.));
#8303=DIRECTION('ref_axis',(1.,0.,0.));
#8304=DIRECTION('center_axis',(0.,1.,0.));
#8305=DIRECTION('ref_axis',(1.,0.,0.));
#8306=DIRECTION('',(0.,1.,0.));
#8307=DIRECTION('center_axis',(0.,-1.,0.));
#8308=DIRECTION('ref_axis',(1.,0.,0.));
#8309=DIRECTION('center_axis',(0.,1.,0.));
#8310=DIRECTION('ref_axis',(1.,0.,0.));
#8311=DIRECTION('center_axis',(0.,1.,0.));
#8312=DIRECTION('ref_axis',(1.,0.,0.));
#8313=DIRECTION('',(0.,1.,0.));
#8314=DIRECTION('center_axis',(0.,-1.,0.));
#8315=DIRECTION('ref_axis',(1.,0.,0.));
#8316=DIRECTION('center_axis',(0.,1.,0.));
#8317=DIRECTION('ref_axis',(1.,0.,0.));
#8318=DIRECTION('center_axis',(0.,1.,0.));
#8319=DIRECTION('ref_axis',(1.,0.,0.));
#8320=DIRECTION('',(0.,1.,0.));
#8321=DIRECTION('center_axis',(0.,-1.,0.));
#8322=DIRECTION('ref_axis',(1.,0.,0.));
#8323=DIRECTION('center_axis',(0.,1.,0.));
#8324=DIRECTION('ref_axis',(1.,0.,0.));
#8325=DIRECTION('center_axis',(0.,1.,0.));
#8326=DIRECTION('ref_axis',(1.,0.,0.));
#8327=DIRECTION('',(0.,-1.,0.));
#8328=DIRECTION('center_axis',(0.,1.,0.));
#8329=DIRECTION('ref_axis',(1.,0.,0.));
#8330=DIRECTION('center_axis',(0.,1.,0.));
#8331=DIRECTION('ref_axis',(1.,0.,0.));
#8332=DIRECTION('center_axis',(0.,-1.,0.));
#8333=DIRECTION('ref_axis',(1.,0.,0.));
#8334=DIRECTION('center_axis',(0.,1.,0.));
#8335=DIRECTION('ref_axis',(1.,0.,0.));
#8336=DIRECTION('center_axis',(0.,-1.,0.));
#8337=DIRECTION('ref_axis',(1.,0.,0.));
#8338=DIRECTION('',(0.,-1.,0.));
#8339=DIRECTION('center_axis',(0.,1.,0.));
#8340=DIRECTION('ref_axis',(1.,0.,0.));
#8341=DIRECTION('center_axis',(0.,1.,0.));
#8342=DIRECTION('ref_axis',(1.,0.,0.));
#8343=DIRECTION('',(0.,-1.,0.));
#8344=DIRECTION('center_axis',(0.,1.,0.));
#8345=DIRECTION('ref_axis',(1.,0.,0.));
#8346=DIRECTION('center_axis',(0.,1.,0.));
#8347=DIRECTION('ref_axis',(1.,0.,0.));
#8348=DIRECTION('center_axis',(0.,1.,0.));
#8349=DIRECTION('ref_axis',(1.,0.,0.));
#8350=DIRECTION('axis',(0.,0.,1.));
#8351=DIRECTION('refdir',(1.,0.,0.));
#8352=DIRECTION('center_axis',(0.,0.,1.));
#8353=DIRECTION('ref_axis',(1.,0.,0.));
#8354=DIRECTION('center_axis',(0.,0.,1.));
#8355=DIRECTION('ref_axis',(1.,0.,0.));
#8356=DIRECTION('',(0.,0.,1.));
#8357=DIRECTION('center_axis',(0.,0.,-1.));
#8358=DIRECTION('ref_axis',(1.,0.,0.));
#8359=DIRECTION('center_axis',(0.,0.,1.));
#8360=DIRECTION('ref_axis',(1.,0.,0.));
#8361=DIRECTION('center_axis',(0.,0.,1.));
#8362=DIRECTION('ref_axis',(1.,0.,0.));
#8363=DIRECTION('center_axis',(0.,0.,1.));
#8364=DIRECTION('ref_axis',(1.,0.,0.));
#8365=DIRECTION('center_axis',(0.,0.,1.));
#8366=DIRECTION('ref_axis',(1.,0.,0.));
#8367=DIRECTION('',(0.,0.,1.));
#8368=DIRECTION('center_axis',(0.,0.,-1.));
#8369=DIRECTION('ref_axis',(1.,0.,0.));
#8370=DIRECTION('center_axis',(0.,0.,1.));
#8371=DIRECTION('ref_axis',(1.,0.,0.));
#8372=DIRECTION('center_axis',(0.,0.,1.));
#8373=DIRECTION('ref_axis',(1.,0.,0.));
#8374=DIRECTION('center_axis',(0.,0.,1.));
#8375=DIRECTION('ref_axis',(1.,0.,0.));
#8376=DIRECTION('center_axis',(0.,0.,1.));
#8377=DIRECTION('ref_axis',(1.,0.,0.));
#8378=DIRECTION('',(0.,0.,1.));
#8379=DIRECTION('center_axis',(0.,0.,-1.));
#8380=DIRECTION('ref_axis',(1.,0.,0.));
#8381=DIRECTION('center_axis',(0.,0.,1.));
#8382=DIRECTION('ref_axis',(1.,0.,0.));
#8383=DIRECTION('center_axis',(0.,0.,1.));
#8384=DIRECTION('ref_axis',(1.,0.,0.));
#8385=DIRECTION('center_axis',(0.,0.,1.));
#8386=DIRECTION('ref_axis',(1.,0.,0.));
#8387=DIRECTION('center_axis',(0.,0.,1.));
#8388=DIRECTION('ref_axis',(1.,0.,0.));
#8389=DIRECTION('',(0.,0.,1.));
#8390=DIRECTION('center_axis',(0.,0.,-1.));
#8391=DIRECTION('ref_axis',(1.,0.,0.));
#8392=DIRECTION('center_axis',(0.,0.,1.));
#8393=DIRECTION('ref_axis',(1.,0.,0.));
#8394=DIRECTION('center_axis',(0.,0.,1.));
#8395=DIRECTION('ref_axis',(1.,0.,0.));
#8396=DIRECTION('center_axis',(0.,0.,1.));
#8397=DIRECTION('ref_axis',(1.,0.,0.));
#8398=DIRECTION('center_axis',(0.,0.,1.));
#8399=DIRECTION('ref_axis',(1.,0.,0.));
#8400=DIRECTION('',(0.,0.,1.));
#8401=DIRECTION('center_axis',(0.,0.,1.));
#8402=DIRECTION('ref_axis',(1.,0.,0.));
#8403=DIRECTION('center_axis',(0.,0.,1.));
#8404=DIRECTION('ref_axis',(1.,0.,0.));
#8405=DIRECTION('',(0.,0.,1.));
#8406=DIRECTION('center_axis',(0.,0.,1.));
#8407=DIRECTION('ref_axis',(1.,0.,0.));
#8408=DIRECTION('center_axis',(0.,0.,1.));
#8409=DIRECTION('ref_axis',(1.,0.,0.));
#8410=DIRECTION('',(0.,0.,1.));
#8411=DIRECTION('center_axis',(0.,0.,1.));
#8412=DIRECTION('ref_axis',(1.,0.,0.));
#8413=DIRECTION('center_axis',(0.,0.,1.));
#8414=DIRECTION('ref_axis',(1.,0.,0.));
#8415=DIRECTION('',(0.,0.,1.));
#8416=DIRECTION('center_axis',(0.,0.,1.));
#8417=DIRECTION('ref_axis',(1.,0.,0.));
#8418=DIRECTION('center_axis',(0.,0.,1.));
#8419=DIRECTION('ref_axis',(1.,0.,0.));
#8420=DIRECTION('',(0.,0.,-1.));
#8421=DIRECTION('center_axis',(0.,0.,1.));
#8422=DIRECTION('ref_axis',(1.,0.,0.));
#8423=DIRECTION('center_axis',(0.,0.,1.));
#8424=DIRECTION('ref_axis',(1.,0.,0.));
#8425=DIRECTION('center_axis',(0.,0.,-1.));
#8426=DIRECTION('ref_axis',(1.,0.,0.));
#8427=DIRECTION('center_axis',(0.,0.,1.));
#8428=DIRECTION('ref_axis',(1.,0.,0.));
#8429=DIRECTION('center_axis',(0.,0.,-1.));
#8430=DIRECTION('ref_axis',(1.,0.,0.));
#8431=DIRECTION('',(0.,0.,-1.));
#8432=DIRECTION('center_axis',(0.,0.,1.));
#8433=DIRECTION('ref_axis',(1.,0.,0.));
#8434=DIRECTION('center_axis',(0.,0.,1.));
#8435=DIRECTION('ref_axis',(1.,0.,0.));
#8436=DIRECTION('',(0.,0.,-1.));
#8437=DIRECTION('center_axis',(0.,0.,1.));
#8438=DIRECTION('ref_axis',(1.,0.,0.));
#8439=DIRECTION('center_axis',(0.,0.,1.));
#8440=DIRECTION('ref_axis',(1.,0.,0.));
#8441=DIRECTION('center_axis',(0.,0.,1.));
#8442=DIRECTION('ref_axis',(1.,0.,0.));
#8443=DIRECTION('axis',(0.,0.,1.));
#8444=DIRECTION('refdir',(1.,0.,0.));
#8445=DIRECTION('center_axis',(0.,1.,0.));
#8446=DIRECTION('ref_axis',(-1.,0.,0.));
#8447=DIRECTION('',(-1.,0.,0.));
#8448=DIRECTION('',(0.,0.,1.));
#8449=DIRECTION('',(-1.,0.,0.));
#8450=DIRECTION('',(0.,0.,1.));
#8451=DIRECTION('center_axis',(1.,0.,0.));
#8452=DIRECTION('ref_axis',(0.,1.,0.));
#8453=DIRECTION('',(0.,1.,0.));
#8454=DIRECTION('',(0.,1.,0.));
#8455=DIRECTION('',(0.,0.,1.));
#8456=DIRECTION('center_axis',(0.,-1.,0.));
#8457=DIRECTION('ref_axis',(1.,0.,0.));
#8458=DIRECTION('',(1.,0.,0.));
#8459=DIRECTION('',(1.,0.,0.));
#8460=DIRECTION('',(0.,0.,1.));
#8461=DIRECTION('center_axis',(-1.,0.,0.));
#8462=DIRECTION('ref_axis',(0.,-1.,0.));
#8463=DIRECTION('',(0.,-1.,0.));
#8464=DIRECTION('',(0.,-1.,0.));
#8465=DIRECTION('center_axis',(0.,0.,1.));
#8466=DIRECTION('ref_axis',(1.,0.,0.));
#8467=DIRECTION('center_axis',(0.,0.,1.));
#8468=DIRECTION('ref_axis',(1.,0.,0.));
#8469=DIRECTION('axis',(0.,0.,1.));
#8470=DIRECTION('refdir',(1.,0.,0.));
#8471=DIRECTION('center_axis',(0.,0.,1.));
#8472=DIRECTION('ref_axis',(1.,0.,0.));
#8473=DIRECTION('center_axis',(0.,0.,1.));
#8474=DIRECTION('ref_axis',(1.,0.,0.));
#8475=DIRECTION('',(0.,0.,1.));
#8476=DIRECTION('center_axis',(0.,0.,1.));
#8477=DIRECTION('ref_axis',(1.,0.,0.));
#8478=DIRECTION('center_axis',(0.,0.,1.));
#8479=DIRECTION('ref_axis',(1.,0.,0.));
#8480=DIRECTION('center_axis',(0.,0.,1.));
#8481=DIRECTION('ref_axis',(1.,0.,0.));
#8482=DIRECTION('center_axis',(0.,0.,1.));
#8483=DIRECTION('ref_axis',(1.,0.,0.));
#8484=DIRECTION('',(0.,0.,1.));
#8485=DIRECTION('center_axis',(0.,0.,1.));
#8486=DIRECTION('ref_axis',(1.,0.,0.));
#8487=DIRECTION('center_axis',(0.,0.,1.));
#8488=DIRECTION('ref_axis',(1.,0.,0.));
#8489=DIRECTION('center_axis',(0.,1.,0.));
#8490=DIRECTION('ref_axis',(-1.,0.,0.));
#8491=DIRECTION('',(-1.,0.,0.));
#8492=DIRECTION('',(0.,0.,1.));
#8493=DIRECTION('',(-1.,0.,0.));
#8494=DIRECTION('',(0.,0.,1.));
#8495=DIRECTION('center_axis',(1.,0.,0.));
#8496=DIRECTION('ref_axis',(0.,1.,0.));
#8497=DIRECTION('',(0.,1.,0.));
#8498=DIRECTION('',(0.,1.,0.));
#8499=DIRECTION('',(0.,0.,1.));
#8500=DIRECTION('center_axis',(0.,-1.,0.));
#8501=DIRECTION('ref_axis',(1.,0.,0.));
#8502=DIRECTION('',(1.,0.,0.));
#8503=DIRECTION('',(1.,0.,0.));
#8504=DIRECTION('',(0.,0.,1.));
#8505=DIRECTION('center_axis',(-1.,0.,0.));
#8506=DIRECTION('ref_axis',(0.,-1.,0.));
#8507=DIRECTION('',(0.,-1.,0.));
#8508=DIRECTION('',(0.,-1.,0.));
#8509=DIRECTION('center_axis',(0.,0.,1.));
#8510=DIRECTION('ref_axis',(1.,0.,0.));
#8511=DIRECTION('center_axis',(0.,0.,1.));
#8512=DIRECTION('ref_axis',(1.,0.,0.));
#8513=DIRECTION('axis',(0.,0.,1.));
#8514=DIRECTION('refdir',(1.,0.,0.));
#8515=DIRECTION('center_axis',(0.,0.,1.));
#8516=DIRECTION('ref_axis',(1.,0.,0.));
#8517=DIRECTION('center_axis',(0.,0.,1.));
#8518=DIRECTION('ref_axis',(1.,0.,0.));
#8519=DIRECTION('',(0.,0.,1.));
#8520=DIRECTION('center_axis',(0.,0.,1.));
#8521=DIRECTION('ref_axis',(1.,0.,0.));
#8522=DIRECTION('center_axis',(0.,0.,1.));
#8523=DIRECTION('ref_axis',(1.,0.,0.));
#8524=DIRECTION('center_axis',(0.,0.,1.));
#8525=DIRECTION('ref_axis',(1.,0.,0.));
#8526=DIRECTION('center_axis',(0.,0.,1.));
#8527=DIRECTION('ref_axis',(1.,0.,0.));
#8528=DIRECTION('',(0.,0.,1.));
#8529=DIRECTION('center_axis',(0.,0.,1.));
#8530=DIRECTION('ref_axis',(1.,0.,0.));
#8531=DIRECTION('center_axis',(0.,0.,1.));
#8532=DIRECTION('ref_axis',(1.,0.,0.));
#8533=DIRECTION('center_axis',(0.,1.,0.));
#8534=DIRECTION('ref_axis',(-1.,0.,0.));
#8535=DIRECTION('',(-1.,0.,0.));
#8536=DIRECTION('',(0.,0.,1.));
#8537=DIRECTION('',(-1.,0.,0.));
#8538=DIRECTION('',(0.,0.,1.));
#8539=DIRECTION('center_axis',(1.,0.,0.));
#8540=DIRECTION('ref_axis',(0.,1.,0.));
#8541=DIRECTION('',(0.,1.,0.));
#8542=DIRECTION('',(0.,1.,0.));
#8543=DIRECTION('',(0.,0.,1.));
#8544=DIRECTION('center_axis',(0.,-1.,0.));
#8545=DIRECTION('ref_axis',(1.,0.,0.));
#8546=DIRECTION('',(1.,0.,0.));
#8547=DIRECTION('',(1.,0.,0.));
#8548=DIRECTION('',(0.,0.,1.));
#8549=DIRECTION('center_axis',(-1.,0.,0.));
#8550=DIRECTION('ref_axis',(0.,-1.,0.));
#8551=DIRECTION('',(0.,-1.,0.));
#8552=DIRECTION('',(0.,-1.,0.));
#8553=DIRECTION('center_axis',(0.,0.,1.));
#8554=DIRECTION('ref_axis',(1.,0.,0.));
#8555=DIRECTION('center_axis',(0.,0.,1.));
#8556=DIRECTION('ref_axis',(1.,0.,0.));
#8557=DIRECTION('axis',(0.,0.,1.));
#8558=DIRECTION('refdir',(1.,0.,0.));
#8559=DIRECTION('center_axis',(0.,1.,0.));
#8560=DIRECTION('ref_axis',(1.,0.,0.));
#8561=DIRECTION('center_axis',(0.,1.,0.));
#8562=DIRECTION('ref_axis',(1.,0.,0.));
#8563=DIRECTION('',(0.,1.,0.));
#8564=DIRECTION('center_axis',(0.,-1.,0.));
#8565=DIRECTION('ref_axis',(1.,0.,0.));
#8566=DIRECTION('center_axis',(0.,1.,0.));
#8567=DIRECTION('ref_axis',(1.,0.,0.));
#8568=DIRECTION('center_axis',(0.,1.,0.));
#8569=DIRECTION('ref_axis',(1.,0.,0.));
#8570=DIRECTION('center_axis',(0.,1.,0.));
#8571=DIRECTION('ref_axis',(1.,0.,0.));
#8572=DIRECTION('center_axis',(0.,1.,0.));
#8573=DIRECTION('ref_axis',(1.,0.,0.));
#8574=DIRECTION('center_axis',(0.,1.,0.));
#8575=DIRECTION('ref_axis',(1.,0.,0.));
#8576=DIRECTION('center_axis',(0.,1.,0.));
#8577=DIRECTION('ref_axis',(1.,0.,0.));
#8578=DIRECTION('',(0.,-1.,0.));
#8579=DIRECTION('center_axis',(0.,1.,0.));
#8580=DIRECTION('ref_axis',(1.,0.,0.));
#8581=DIRECTION('center_axis',(0.,1.,0.));
#8582=DIRECTION('ref_axis',(1.,0.,0.));
#8583=DIRECTION('',(0.,-1.,0.));
#8584=DIRECTION('center_axis',(0.,1.,0.));
#8585=DIRECTION('ref_axis',(1.,0.,0.));
#8586=DIRECTION('center_axis',(0.,1.,0.));
#8587=DIRECTION('ref_axis',(1.,0.,0.));
#8588=DIRECTION('axis',(0.,0.,1.));
#8589=DIRECTION('refdir',(1.,0.,0.));
#8590=DIRECTION('center_axis',(0.866025403784439,0.,-0.5));
#8591=DIRECTION('ref_axis',(0.5,0.,0.866025403784439));
#8592=DIRECTION('',(-0.5,0.,-0.866025403784439));
#8593=DIRECTION('',(0.,-1.,0.));
#8594=DIRECTION('',(0.5,0.,0.866025403784439));
#8595=DIRECTION('',(0.,-1.,0.));
#8596=DIRECTION('center_axis',(1.20185167898973E-16,0.,-1.));
#8597=DIRECTION('ref_axis',(1.,0.,1.20185167898973E-16));
#8598=DIRECTION('',(-1.,0.,-1.20185167898973E-16));
#8599=DIRECTION('',(0.,-1.,0.));
#8600=DIRECTION('',(1.,0.,1.20185167898973E-16));
#8601=DIRECTION('center_axis',(-0.866025403784439,0.,-0.5));
#8602=DIRECTION('ref_axis',(0.5,0.,-0.866025403784439));
#8603=DIRECTION('',(-0.5,0.,0.866025403784439));
#8604=DIRECTION('',(0.,-1.,0.));
#8605=DIRECTION('',(0.5,0.,-0.866025403784439));
#8606=DIRECTION('center_axis',(-0.866025403784439,0.,0.5));
#8607=DIRECTION('ref_axis',(-0.5,0.,-0.866025403784439));
#8608=DIRECTION('',(0.5,0.,0.866025403784439));
#8609=DIRECTION('',(0.,-1.,0.));
#8610=DIRECTION('',(-0.5,0.,-0.866025403784439));
#8611=DIRECTION('center_axis',(-2.40370335797945E-16,0.,1.));
#8612=DIRECTION('ref_axis',(-1.,0.,-2.40370335797945E-16));
#8613=DIRECTION('',(1.,0.,2.40370335797945E-16));
#8614=DIRECTION('',(0.,-1.,0.));
#8615=DIRECTION('',(-1.,0.,-2.40370335797945E-16));
#8616=DIRECTION('center_axis',(0.866025403784439,0.,0.5));
#8617=DIRECTION('ref_axis',(-0.5,0.,0.866025403784439));
#8618=DIRECTION('',(0.5,0.,-0.866025403784439));
#8619=DIRECTION('',(-0.5,0.,0.866025403784439));
#8620=DIRECTION('center_axis',(0.,1.,0.));
#8621=DIRECTION('ref_axis',(1.,0.,0.));
#8622=DIRECTION('center_axis',(0.,-1.,0.));
#8623=DIRECTION('ref_axis',(0.,0.,-1.));
#8624=DIRECTION('center_axis',(0.,1.,0.));
#8625=DIRECTION('ref_axis',(1.,0.,0.));
#8626=DIRECTION('center_axis',(0.,1.,0.));
#8627=DIRECTION('ref_axis',(1.,0.,0.));
#8628=DIRECTION('center_axis',(0.,1.,0.));
#8629=DIRECTION('ref_axis',(0.,0.,1.));
#8630=DIRECTION('center_axis',(0.,-1.,0.));
#8631=DIRECTION('ref_axis',(1.,0.,0.));
#8632=DIRECTION('center_axis',(0.,-1.,0.));
#8633=DIRECTION('ref_axis',(1.,0.,0.));
#8634=DIRECTION('center_axis',(0.,-1.,0.));
#8635=DIRECTION('ref_axis',(1.,0.,0.));
#8636=DIRECTION('',(0.707106781186548,0.707106781186547,8.65956056235493E-17));
#8637=DIRECTION('center_axis',(0.,-1.,0.));
#8638=DIRECTION('ref_axis',(1.,0.,0.));
#8639=DIRECTION('center_axis',(0.,-1.,0.));
#8640=DIRECTION('ref_axis',(1.,0.,0.));
#8641=DIRECTION('',(0.,1.,0.));
#8642=DIRECTION('center_axis',(0.,1.,0.));
#8643=DIRECTION('ref_axis',(1.,0.,0.));
#8644=DIRECTION('center_axis',(0.,-1.,0.));
#8645=DIRECTION('ref_axis',(1.,0.,0.));
#8646=DIRECTION('',(-0.707106781186547,0.707106781186548,-8.65956056235493E-17));
#8647=DIRECTION('center_axis',(0.,-1.,0.));
#8648=DIRECTION('ref_axis',(0.,0.,-1.));
#8649=DIRECTION('center_axis',(0.,-1.,0.));
#8650=DIRECTION('ref_axis',(1.,0.,0.));
#8651=DIRECTION('center_axis',(0.,1.,0.));
#8652=DIRECTION('ref_axis',(1.,0.,0.));
#8653=DIRECTION('center_axis',(0.,1.,0.));
#8654=DIRECTION('ref_axis',(1.,0.,0.));
#8655=DIRECTION('',(-0.447213595499958,0.894427190999916,-5.47678698264203E-17));
#8656=DIRECTION('center_axis',(0.,-1.,0.));
#8657=DIRECTION('ref_axis',(1.,0.,0.));
#8658=DIRECTION('',(0.,1.,0.));
#8659=DIRECTION('axis',(0.,0.,1.));
#8660=DIRECTION('refdir',(1.,0.,0.));
#8661=DIRECTION('axis',(0.,0.,1.));
#8662=DIRECTION('refdir',(1.,0.,0.));
#8663=DIRECTION('center_axis',(0.,-1.,0.));
#8664=DIRECTION('ref_axis',(0.,0.,-1.));
#8665=DIRECTION('center_axis',(0.,-1.,0.));
#8666=DIRECTION('ref_axis',(1.,0.,0.));
#8667=DIRECTION('center_axis',(0.,-1.,0.));
#8668=DIRECTION('ref_axis',(1.,0.,0.));
#8669=DIRECTION('center_axis',(1.,0.,1.22464679914735E-16));
#8670=DIRECTION('ref_axis',(-1.22464679914735E-16,0.,1.));
#8671=DIRECTION('center_axis',(0.,1.,0.));
#8672=DIRECTION('ref_axis',(1.,0.,0.));
#8673=DIRECTION('center_axis',(0.,1.,0.));
#8674=DIRECTION('ref_axis',(1.,0.,0.));
#8675=DIRECTION('center_axis',(0.,-1.,0.));
#8676=DIRECTION('ref_axis',(1.,0.,0.));
#8677=DIRECTION('',(0.,1.,0.));
#8678=DIRECTION('center_axis',(0.,-1.,0.));
#8679=DIRECTION('ref_axis',(1.,0.,0.));
#8680=DIRECTION('center_axis',(0.,-1.,0.));
#8681=DIRECTION('ref_axis',(1.,0.,0.));
#8682=DIRECTION('center_axis',(0.,-1.,0.));
#8683=DIRECTION('ref_axis',(1.,0.,0.));
#8684=DIRECTION('',(0.,1.,0.));
#8685=DIRECTION('center_axis',(0.,-1.,0.));
#8686=DIRECTION('ref_axis',(1.,0.,0.));
#8687=DIRECTION('center_axis',(0.,1.,0.));
#8688=DIRECTION('ref_axis',(1.,0.,0.));
#8689=DIRECTION('',(-0.707106781186547,0.707106781186548,-8.65956056235493E-17));
#8690=DIRECTION('center_axis',(0.,-1.,0.));
#8691=DIRECTION('ref_axis',(1.,0.,0.));
#8692=DIRECTION('center_axis',(0.,1.,0.));
#8693=DIRECTION('ref_axis',(0.,0.,1.));
#8694=DIRECTION('center_axis',(0.,-1.,0.));
#8695=DIRECTION('ref_axis',(1.,0.,0.));
#8696=DIRECTION('center_axis',(0.,-1.,0.));
#8697=DIRECTION('ref_axis',(1.,0.,0.));
#8698=DIRECTION('',(0.,1.,0.));
#8699=DIRECTION('center_axis',(0.,-1.,0.));
#8700=DIRECTION('ref_axis',(0.,0.,-1.));
#8701=DIRECTION('center_axis',(0.,-1.,0.));
#8702=DIRECTION('ref_axis',(1.,0.,0.));
#8703=DIRECTION('center_axis',(0.,-1.,0.));
#8704=DIRECTION('ref_axis',(1.,0.,0.));
#8705=DIRECTION('',(0.707106781186547,0.707106781186548,8.65956056235493E-17));
#8706=DIRECTION('axis',(0.,0.,1.));
#8707=DIRECTION('refdir',(1.,0.,0.));
#8708=DIRECTION('center_axis',(0.,-1.,0.));
#8709=DIRECTION('ref_axis',(0.,0.,-1.));
#8710=DIRECTION('center_axis',(0.,-1.,0.));
#8711=DIRECTION('ref_axis',(1.,0.,0.));
#8712=DIRECTION('center_axis',(0.,-1.,0.));
#8713=DIRECTION('ref_axis',(1.,0.,0.));
#8714=DIRECTION('center_axis',(1.,0.,1.22464679914735E-16));
#8715=DIRECTION('ref_axis',(-1.22464679914735E-16,0.,1.));
#8716=DIRECTION('center_axis',(0.,1.,0.));
#8717=DIRECTION('ref_axis',(1.,0.,0.));
#8718=DIRECTION('center_axis',(0.,1.,0.));
#8719=DIRECTION('ref_axis',(1.,0.,0.));
#8720=DIRECTION('center_axis',(0.,-1.,0.));
#8721=DIRECTION('ref_axis',(1.,0.,0.));
#8722=DIRECTION('center_axis',(0.,-1.,0.));
#8723=DIRECTION('ref_axis',(1.,0.,0.));
#8724=DIRECTION('',(0.,1.,0.));
#8725=DIRECTION('center_axis',(0.,1.,0.));
#8726=DIRECTION('ref_axis',(0.,0.,1.));
#8727=DIRECTION('center_axis',(0.,-1.,0.));
#8728=DIRECTION('ref_axis',(1.,0.,0.));
#8729=DIRECTION('center_axis',(0.,-1.,0.));
#8730=DIRECTION('ref_axis',(1.,0.,0.));
#8731=DIRECTION('center_axis',(0.,-1.,0.));
#8732=DIRECTION('ref_axis',(1.,0.,0.));
#8733=DIRECTION('center_axis',(0.,-1.,0.));
#8734=DIRECTION('ref_axis',(1.,0.,0.));
#8735=DIRECTION('',(0.707106781186548,0.707106781186547,8.65956056235494E-17));
#8736=DIRECTION('center_axis',(0.,-1.,0.));
#8737=DIRECTION('ref_axis',(1.,0.,0.));
#8738=DIRECTION('center_axis',(0.,-1.,0.));
#8739=DIRECTION('ref_axis',(1.,0.,0.));
#8740=DIRECTION('',(0.,1.,0.));
#8741=DIRECTION('center_axis',(0.,1.,0.));
#8742=DIRECTION('ref_axis',(1.,0.,0.));
#8743=DIRECTION('center_axis',(0.,-1.,0.));
#8744=DIRECTION('ref_axis',(1.,0.,0.));
#8745=DIRECTION('',(-0.707106781186548,0.707106781186547,-8.65956056235494E-17));
#8746=DIRECTION('center_axis',(0.,-1.,0.));
#8747=DIRECTION('ref_axis',(0.,0.,-1.));
#8748=DIRECTION('center_axis',(0.,-1.,0.));
#8749=DIRECTION('ref_axis',(1.,0.,0.));
#8750=DIRECTION('',(0.,1.,0.));
#8751=DIRECTION('axis',(0.,0.,1.));
#8752=DIRECTION('refdir',(1.,0.,0.));
#8753=DIRECTION('center_axis',(0.,0.,1.));
#8754=DIRECTION('ref_axis',(1.,0.,0.));
#8755=DIRECTION('center_axis',(1.22464679914735E-16,-1.,0.));
#8756=DIRECTION('ref_axis',(-1.,-1.22464679914735E-16,0.));
#8757=DIRECTION('center_axis',(0.707106781186548,0.,0.707106781186548));
#8758=DIRECTION('ref_axis',(0.707106781186548,0.,-0.707106781186548));
#8759=DIRECTION('center_axis',(8.65956056235494E-17,-1.,-8.65956056235493E-17));
#8760=DIRECTION('ref_axis',(-0.707106781186547,-1.22464679914735E-16,0.707106781186547));
#8761=DIRECTION('center_axis',(1.,0.,0.));
#8762=DIRECTION('ref_axis',(6.12323399573676E-17,0.,-1.));
#8763=DIRECTION('center_axis',(7.49879891330929E-33,-1.,-1.22464679914735E-16));
#8764=DIRECTION('ref_axis',(-6.12323399573676E-17,-1.22464679914735E-16,
1.));
#8765=DIRECTION('center_axis',(0.707106781186548,0.,-0.707106781186548));
#8766=DIRECTION('ref_axis',(-0.707106781186548,0.,-0.707106781186548));
#8767=DIRECTION('center_axis',(-8.65956056235493E-17,-1.,-8.65956056235494E-17));
#8768=DIRECTION('ref_axis',(0.707106781186547,-1.22464679914735E-16,0.707106781186547));
#8769=DIRECTION('center_axis',(0.,0.,-1.));
#8770=DIRECTION('ref_axis',(-1.,0.,-1.22464679914735E-16));
#8771=DIRECTION('center_axis',(-1.22464679914735E-16,-1.,-1.49975978266186E-32));
#8772=DIRECTION('ref_axis',(1.,-1.22464679914735E-16,1.22464679914735E-16));
#8773=DIRECTION('center_axis',(-0.707106781186547,0.,-0.707106781186548));
#8774=DIRECTION('ref_axis',(-0.707106781186548,0.,0.707106781186547));
#8775=DIRECTION('center_axis',(-8.65956056235493E-17,-1.,8.65956056235493E-17));
#8776=DIRECTION('ref_axis',(0.707106781186548,-1.22464679914735E-16,-0.707106781186547));
#8777=DIRECTION('center_axis',(-1.,0.,0.));
#8778=DIRECTION('ref_axis',(-1.83697019872103E-16,0.,1.));
#8779=DIRECTION('center_axis',(-2.24963967399279E-32,-1.,1.22464679914735E-16));
#8780=DIRECTION('ref_axis',(1.83697019872103E-16,-1.22464679914735E-16,
-1.));
#8781=DIRECTION('center_axis',(-0.707106781186548,0.,0.707106781186548));
#8782=DIRECTION('ref_axis',(0.707106781186547,0.,0.707106781186548));
#8783=DIRECTION('center_axis',(8.65956056235493E-17,-1.,8.65956056235493E-17));
#8784=DIRECTION('ref_axis',(-0.707106781186547,-1.22464679914735E-16,-0.707106781186548));
#8785=DIRECTION('axis',(0.,0.,1.));
#8786=DIRECTION('refdir',(1.,0.,0.));
#8787=DIRECTION('center_axis',(0.,0.,1.));
#8788=DIRECTION('ref_axis',(1.,0.,0.));
#8789=DIRECTION('center_axis',(0.,-1.,0.));
#8790=DIRECTION('ref_axis',(0.,0.,-1.));
#8791=DIRECTION('center_axis',(0.,-1.,0.));
#8792=DIRECTION('ref_axis',(0.,0.,-1.));
#8793=DIRECTION('center_axis',(0.,1.,0.));
#8794=DIRECTION('ref_axis',(1.,0.,0.));
#8795=DIRECTION('center_axis',(0.,1.,0.));
#8796=DIRECTION('ref_axis',(1.,0.,0.));
#8797=DIRECTION('center_axis',(0.,1.,0.));
#8798=DIRECTION('ref_axis',(1.,0.,0.));
#8799=DIRECTION('center_axis',(0.,1.,0.));
#8800=DIRECTION('ref_axis',(1.,0.,0.));
#8801=DIRECTION('',(0.,-1.,0.));
#8802=DIRECTION('center_axis',(0.,-1.,0.));
#8803=DIRECTION('ref_axis',(1.,0.,0.));
#8804=DIRECTION('center_axis',(0.,1.,0.));
#8805=DIRECTION('ref_axis',(1.,0.,0.));
#8806=DIRECTION('center_axis',(0.,1.,0.));
#8807=DIRECTION('ref_axis',(1.,0.,0.));
#8808=DIRECTION('center_axis',(0.,1.,0.));
#8809=DIRECTION('ref_axis',(1.,0.,0.));
#8810=DIRECTION('center_axis',(0.,1.,0.));
#8811=DIRECTION('ref_axis',(1.,0.,0.));
#8812=DIRECTION('center_axis',(0.,1.,0.));
#8813=DIRECTION('ref_axis',(1.,0.,0.));
#8814=DIRECTION('center_axis',(0.,1.,0.));
#8815=DIRECTION('ref_axis',(1.,0.,0.));
#8816=DIRECTION('center_axis',(0.,-1.,0.));
#8817=DIRECTION('ref_axis',(1.,0.,0.));
#8818=DIRECTION('center_axis',(0.,-1.,0.));
#8819=DIRECTION('ref_axis',(0.,0.,-1.));
#8820=DIRECTION('center_axis',(6.12323399573677E-17,0.,1.));
#8821=DIRECTION('ref_axis',(1.,0.,0.));
#8822=DIRECTION('center_axis',(0.,-1.,0.));
#8823=DIRECTION('ref_axis',(0.,0.,-1.));
#8824=DIRECTION('center_axis',(0.,1.,0.));
#8825=DIRECTION('ref_axis',(1.,0.,0.));
#8826=DIRECTION('center_axis',(0.,-1.,0.));
#8827=DIRECTION('ref_axis',(1.,0.,0.));
#8828=DIRECTION('center_axis',(0.,-1.,0.));
#8829=DIRECTION('ref_axis',(0.,0.,-1.));
#8830=DIRECTION('center_axis',(0.,0.,1.));
#8831=DIRECTION('ref_axis',(1.,0.,0.));
#8832=DIRECTION('center_axis',(0.,-1.,0.));
#8833=DIRECTION('ref_axis',(0.,0.,-1.));
#8834=DIRECTION('center_axis',(0.,1.,0.));
#8835=DIRECTION('ref_axis',(1.,0.,0.));
#8836=DIRECTION('center_axis',(0.,-1.,0.));
#8837=DIRECTION('ref_axis',(1.,0.,0.));
#8838=DIRECTION('center_axis',(0.,-1.,0.));
#8839=DIRECTION('ref_axis',(0.,0.,-1.));
#8840=DIRECTION('center_axis',(0.,0.,1.));
#8841=DIRECTION('ref_axis',(1.,0.,0.));
#8842=DIRECTION('center_axis',(0.,-1.,0.));
#8843=DIRECTION('ref_axis',(0.,0.,-1.));
#8844=DIRECTION('center_axis',(0.,1.,0.));
#8845=DIRECTION('ref_axis',(1.,0.,0.));
#8846=DIRECTION('center_axis',(0.,-1.,0.));
#8847=DIRECTION('ref_axis',(1.,0.,0.));
#8848=DIRECTION('center_axis',(0.,-1.,0.));
#8849=DIRECTION('ref_axis',(0.,0.,-1.));
#8850=DIRECTION('center_axis',(0.,0.,1.));
#8851=DIRECTION('ref_axis',(1.,0.,0.));
#8852=DIRECTION('center_axis',(0.,-1.,0.));
#8853=DIRECTION('ref_axis',(0.,0.,-1.));
#8854=DIRECTION('center_axis',(0.,1.,0.));
#8855=DIRECTION('ref_axis',(1.,0.,0.));
#8856=DIRECTION('center_axis',(0.,-1.,0.));
#8857=DIRECTION('ref_axis',(1.,0.,0.));
#8858=DIRECTION('center_axis',(0.,-1.,0.));
#8859=DIRECTION('ref_axis',(0.,0.,-1.));
#8860=DIRECTION('center_axis',(6.12323399573676E-17,0.,1.));
#8861=DIRECTION('ref_axis',(1.,0.,0.));
#8862=DIRECTION('center_axis',(0.,-1.,0.));
#8863=DIRECTION('ref_axis',(0.,0.,-1.));
#8864=DIRECTION('center_axis',(0.,1.,0.));
#8865=DIRECTION('ref_axis',(1.,0.,0.));
#8866=DIRECTION('center_axis',(0.,-1.,0.));
#8867=DIRECTION('ref_axis',(1.,0.,0.));
#8868=DIRECTION('center_axis',(0.,-1.,0.));
#8869=DIRECTION('ref_axis',(0.,0.,-1.));
#8870=DIRECTION('center_axis',(0.,0.,1.));
#8871=DIRECTION('ref_axis',(1.,0.,0.));
#8872=DIRECTION('center_axis',(0.,-1.,0.));
#8873=DIRECTION('ref_axis',(0.,0.,-1.));
#8874=DIRECTION('center_axis',(0.,1.,0.));
#8875=DIRECTION('ref_axis',(1.,0.,0.));
#8876=DIRECTION('center_axis',(0.,1.,0.));
#8877=DIRECTION('ref_axis',(1.,0.,0.));
#8878=DIRECTION('',(0.,1.,0.));
#8879=DIRECTION('center_axis',(0.,-1.,0.));
#8880=DIRECTION('ref_axis',(1.,0.,0.));
#8881=DIRECTION('center_axis',(0.,-1.,0.));
#8882=DIRECTION('ref_axis',(1.,0.,0.));
#8883=DIRECTION('center_axis',(0.,1.,0.));
#8884=DIRECTION('ref_axis',(1.,0.,0.));
#8885=DIRECTION('center_axis',(0.,-1.,0.));
#8886=DIRECTION('ref_axis',(0.,0.,-1.));
#8887=DIRECTION('center_axis',(0.,0.,1.));
#8888=DIRECTION('ref_axis',(1.,0.,0.));
#8889=DIRECTION('center_axis',(0.,-1.,0.));
#8890=DIRECTION('ref_axis',(0.,0.,-1.));
#8891=DIRECTION('center_axis',(0.,-1.,0.));
#8892=DIRECTION('ref_axis',(-1.,0.,0.));
#8893=DIRECTION('center_axis',(0.,1.,0.));
#8894=DIRECTION('ref_axis',(1.,0.,0.));
#8895=DIRECTION('axis',(0.,0.,1.));
#8896=DIRECTION('refdir',(1.,0.,0.));
#8897=DIRECTION('center_axis',(0.,1.,0.));
#8898=DIRECTION('ref_axis',(0.,0.,1.));
#8899=DIRECTION('center_axis',(0.,-1.,0.));
#8900=DIRECTION('ref_axis',(1.,0.,0.));
#8901=DIRECTION('center_axis',(0.,-1.,0.));
#8902=DIRECTION('ref_axis',(1.,0.,0.));
#8903=DIRECTION('center_axis',(0.,-1.,0.));
#8904=DIRECTION('ref_axis',(1.,0.,0.));
#8905=DIRECTION('center_axis',(0.,-1.,0.));
#8906=DIRECTION('ref_axis',(1.,0.,0.));
#8907=DIRECTION('',(0.,1.,0.));
#8908=DIRECTION('center_axis',(0.,-1.,0.));
#8909=DIRECTION('ref_axis',(0.,0.,-1.));
#8910=DIRECTION('center_axis',(0.,-1.,0.));
#8911=DIRECTION('ref_axis',(1.,0.,0.));
#8912=DIRECTION('center_axis',(0.,-1.,0.));
#8913=DIRECTION('ref_axis',(1.,0.,0.));
#8914=DIRECTION('',(0.,1.,0.));
#8915=DIRECTION('center_axis',(0.,1.,0.));
#8916=DIRECTION('ref_axis',(0.,0.,1.));
#8917=DIRECTION('center_axis',(0.,-1.,0.));
#8918=DIRECTION('ref_axis',(1.,0.,0.));
#8919=DIRECTION('center_axis',(0.,-1.,0.));
#8920=DIRECTION('ref_axis',(1.,0.,0.));
#8921=DIRECTION('center_axis',(0.,-1.,0.));
#8922=DIRECTION('ref_axis',(1.,0.,0.));
#8923=DIRECTION('center_axis',(0.,-1.,0.));
#8924=DIRECTION('ref_axis',(1.,0.,0.));
#8925=DIRECTION('',(0.,1.,0.));
#8926=DIRECTION('center_axis',(0.,-1.,0.));
#8927=DIRECTION('ref_axis',(0.,0.,-1.));
#8928=DIRECTION('center_axis',(0.,-1.,0.));
#8929=DIRECTION('ref_axis',(1.,0.,0.));
#8930=DIRECTION('center_axis',(0.,-1.,0.));
#8931=DIRECTION('ref_axis',(1.,0.,0.));
#8932=DIRECTION('',(0.,1.,0.));
#8933=DIRECTION('',(0.,0.,1.));
#8934=DIRECTION('',(1.,0.,0.));
#8935=DIRECTION('',(0.,0.,1.));
#8936=DIRECTION('',(1.,0.,0.));
#8937=DIRECTION('',(0.,0.,1.));
#8938=DIRECTION('',(1.,0.,0.));
#8939=DIRECTION('',(0.,0.,1.));
#8940=DIRECTION('',(1.,0.,0.));
#8941=DIRECTION('',(0.,0.,1.));
#8942=DIRECTION('',(1.,0.,0.));
#8943=DIRECTION('axis',(0.,0.,1.));
#8944=DIRECTION('refdir',(1.,0.,0.));
#8945=DIRECTION('axis',(0.,0.,1.));
#8946=DIRECTION('refdir',(1.,0.,0.));
#8947=DIRECTION('center_axis',(0.,1.,0.));
#8948=DIRECTION('ref_axis',(0.,0.,1.));
#8949=DIRECTION('center_axis',(0.,-1.,0.));
#8950=DIRECTION('ref_axis',(1.,0.,0.));
#8951=DIRECTION('',(-1.,0.,0.));
#8952=DIRECTION('',(0.,0.,-1.));
#8953=DIRECTION('',(1.,0.,0.));
#8954=DIRECTION('center_axis',(0.,0.,1.));
#8955=DIRECTION('ref_axis',(1.,0.,0.));
#8956=DIRECTION('',(0.,-1.,0.));
#8957=DIRECTION('',(0.,1.,0.));
#8958=DIRECTION('',(-1.,0.,0.));
#8959=DIRECTION('center_axis',(0.,-1.,0.));
#8960=DIRECTION('ref_axis',(0.,0.,-1.));
#8961=DIRECTION('center_axis',(0.,1.,0.));
#8962=DIRECTION('ref_axis',(1.,0.,0.));
#8963=DIRECTION('',(0.,0.,1.));
#8964=DIRECTION('',(1.,0.,0.));
#8965=DIRECTION('center_axis',(0.,0.,-1.));
#8966=DIRECTION('ref_axis',(-1.,0.,0.));
#8967=DIRECTION('',(0.,1.,0.));
#8968=DIRECTION('',(0.,1.,0.));
#8969=DIRECTION('center_axis',(1.,0.,0.));
#8970=DIRECTION('ref_axis',(0.,0.,-1.));
#8971=DIRECTION('center_axis',(0.,1.,0.));
#8972=DIRECTION('ref_axis',(0.,0.,1.));
#8973=DIRECTION('center_axis',(0.,-1.,0.));
#8974=DIRECTION('ref_axis',(1.,0.,0.));
#8975=DIRECTION('center_axis',(0.,-1.,0.));
#8976=DIRECTION('ref_axis',(1.,0.,0.));
#8977=DIRECTION('center_axis',(0.,-1.,0.));
#8978=DIRECTION('ref_axis',(1.,0.,0.));
#8979=DIRECTION('center_axis',(0.,-1.,0.));
#8980=DIRECTION('ref_axis',(1.,0.,0.));
#8981=DIRECTION('',(0.,1.,0.));
#8982=DIRECTION('center_axis',(0.,-1.,0.));
#8983=DIRECTION('ref_axis',(0.,0.,-1.));
#8984=DIRECTION('center_axis',(0.,-1.,0.));
#8985=DIRECTION('ref_axis',(1.,0.,0.));
#8986=DIRECTION('center_axis',(0.,-1.,0.));
#8987=DIRECTION('ref_axis',(1.,0.,0.));
#8988=DIRECTION('center_axis',(0.,-1.,0.));
#8989=DIRECTION('ref_axis',(1.,0.,0.));
#8990=DIRECTION('',(0.,1.,0.));
#8991=DIRECTION('center_axis',(0.,1.,0.));
#8992=DIRECTION('ref_axis',(0.,0.,1.));
#8993=DIRECTION('center_axis',(0.,-1.,0.));
#8994=DIRECTION('ref_axis',(1.,0.,0.));
#8995=DIRECTION('center_axis',(0.,-1.,0.));
#8996=DIRECTION('ref_axis',(1.,0.,0.));
#8997=DIRECTION('center_axis',(0.,-1.,0.));
#8998=DIRECTION('ref_axis',(1.,0.,0.));
#8999=DIRECTION('',(0.,1.,0.));
#9000=DIRECTION('center_axis',(0.,-1.,0.));
#9001=DIRECTION('ref_axis',(0.,0.,-1.));
#9002=DIRECTION('center_axis',(0.,-1.,0.));
#9003=DIRECTION('ref_axis',(1.,0.,0.));
#9004=DIRECTION('center_axis',(0.,-1.,0.));
#9005=DIRECTION('ref_axis',(1.,0.,0.));
#9006=DIRECTION('center_axis',(0.,-1.,0.));
#9007=DIRECTION('ref_axis',(1.,0.,0.));
#9008=DIRECTION('',(0.,1.,0.));
#9009=DIRECTION('center_axis',(0.,1.,0.));
#9010=DIRECTION('ref_axis',(0.,0.,1.));
#9011=DIRECTION('center_axis',(0.,-1.,0.));
#9012=DIRECTION('ref_axis',(1.,0.,0.));
#9013=DIRECTION('center_axis',(0.,-1.,0.));
#9014=DIRECTION('ref_axis',(1.,0.,0.));
#9015=DIRECTION('center_axis',(0.,-1.,0.));
#9016=DIRECTION('ref_axis',(1.,0.,0.));
#9017=DIRECTION('',(0.,1.,0.));
#9018=DIRECTION('center_axis',(0.,-1.,0.));
#9019=DIRECTION('ref_axis',(0.,0.,-1.));
#9020=DIRECTION('center_axis',(0.,-1.,0.));
#9021=DIRECTION('ref_axis',(1.,0.,0.));
#9022=DIRECTION('center_axis',(0.,-1.,0.));
#9023=DIRECTION('ref_axis',(1.,0.,0.));
#9024=DIRECTION('',(0.,1.,0.));
#9025=DIRECTION('axis',(0.,0.,1.));
#9026=DIRECTION('refdir',(1.,0.,0.));
#9027=DIRECTION('center_axis',(0.,1.,0.));
#9028=DIRECTION('ref_axis',(0.,0.,1.));
#9029=DIRECTION('center_axis',(0.,1.,0.));
#9030=DIRECTION('ref_axis',(1.,0.,0.));
#9031=DIRECTION('',(1.,0.,0.));
#9032=DIRECTION('center_axis',(0.,-1.,0.));
#9033=DIRECTION('ref_axis',(1.,0.,0.));
#9034=DIRECTION('',(-1.,0.,0.));
#9035=DIRECTION('center_axis',(0.,0.,-1.));
#9036=DIRECTION('ref_axis',(-1.,0.,0.));
#9037=DIRECTION('',(0.,-1.,0.));
#9038=DIRECTION('',(0.,1.,0.));
#9039=DIRECTION('',(1.,0.,0.));
#9040=DIRECTION('center_axis',(0.,-1.,0.));
#9041=DIRECTION('ref_axis',(0.,0.,-1.));
#9042=DIRECTION('center_axis',(0.,-1.,0.));
#9043=DIRECTION('ref_axis',(1.,0.,0.));
#9044=DIRECTION('center_axis',(0.,1.,0.));
#9045=DIRECTION('ref_axis',(1.,0.,0.));
#9046=DIRECTION('',(-1.,0.,0.));
#9047=DIRECTION('center_axis',(0.,0.,1.));
#9048=DIRECTION('ref_axis',(1.,0.,0.));
#9049=DIRECTION('',(0.,1.,0.));
#9050=DIRECTION('',(0.,-1.,0.));
#9051=DIRECTION('center_axis',(0.,1.,0.));
#9052=DIRECTION('ref_axis',(0.,0.,1.));
#9053=DIRECTION('center_axis',(0.,-1.,0.));
#9054=DIRECTION('ref_axis',(1.,0.,0.));
#9055=DIRECTION('center_axis',(0.,-1.,0.));
#9056=DIRECTION('ref_axis',(1.,0.,0.));
#9057=DIRECTION('center_axis',(0.,-1.,0.));
#9058=DIRECTION('ref_axis',(1.,0.,0.));
#9059=DIRECTION('center_axis',(0.,-1.,0.));
#9060=DIRECTION('ref_axis',(1.,0.,0.));
#9061=DIRECTION('',(0.,1.,0.));
#9062=DIRECTION('center_axis',(0.,-1.,0.));
#9063=DIRECTION('ref_axis',(0.,0.,-1.));
#9064=DIRECTION('center_axis',(0.,-1.,0.));
#9065=DIRECTION('ref_axis',(1.,0.,0.));
#9066=DIRECTION('center_axis',(0.,-1.,0.));
#9067=DIRECTION('ref_axis',(1.,0.,0.));
#9068=DIRECTION('',(0.,1.,0.));
#9069=DIRECTION('',(0.,0.,1.));
#9070=DIRECTION('',(1.,0.,0.));
#9071=DIRECTION('',(0.,0.,1.));
#9072=DIRECTION('',(1.,0.,0.));
#9073=DIRECTION('axis',(0.,0.,1.));
#9074=DIRECTION('refdir',(1.,0.,0.));
#9075=DIRECTION('center_axis',(0.866025403784439,0.,-0.5));
#9076=DIRECTION('ref_axis',(0.5,0.,0.866025403784439));
#9077=DIRECTION('',(-0.5,0.,-0.866025403784439));
#9078=DIRECTION('',(0.,-1.,0.));
#9079=DIRECTION('',(0.5,0.,0.866025403784439));
#9080=DIRECTION('',(0.,-1.,0.));
#9081=DIRECTION('center_axis',(1.60246890531964E-16,0.,-1.));
#9082=DIRECTION('ref_axis',(1.,0.,1.60246890531964E-16));
#9083=DIRECTION('',(-1.,0.,-1.60246890531964E-16));
#9084=DIRECTION('',(0.,-1.,0.));
#9085=DIRECTION('',(1.,0.,1.60246890531964E-16));
#9086=DIRECTION('center_axis',(-0.866025403784439,0.,-0.5));
#9087=DIRECTION('ref_axis',(0.5,0.,-0.866025403784439));
#9088=DIRECTION('',(-0.5,0.,0.866025403784439));
#9089=DIRECTION('',(0.,-1.,0.));
#9090=DIRECTION('',(0.5,0.,-0.866025403784439));
#9091=DIRECTION('center_axis',(-0.866025403784439,0.,0.5));
#9092=DIRECTION('ref_axis',(-0.5,0.,-0.866025403784439));
#9093=DIRECTION('',(0.5,0.,0.866025403784439));
#9094=DIRECTION('',(0.,-1.,0.));
#9095=DIRECTION('',(-0.5,0.,-0.866025403784439));
#9096=DIRECTION('center_axis',(-1.60246890531964E-16,0.,1.));
#9097=DIRECTION('ref_axis',(-1.,0.,-1.60246890531964E-16));
#9098=DIRECTION('',(1.,0.,1.60246890531964E-16));
#9099=DIRECTION('',(0.,-1.,0.));
#9100=DIRECTION('',(-1.,0.,-1.60246890531964E-16));
#9101=DIRECTION('center_axis',(0.866025403784439,0.,0.5));
#9102=DIRECTION('ref_axis',(-0.5,0.,0.866025403784439));
#9103=DIRECTION('',(0.5,0.,-0.866025403784439));
#9104=DIRECTION('',(-0.5,0.,0.866025403784439));
#9105=DIRECTION('center_axis',(0.,1.,0.));
#9106=DIRECTION('ref_axis',(1.,0.,0.));
#9107=DIRECTION('center_axis',(0.,-1.,0.));
#9108=DIRECTION('ref_axis',(0.,0.,-1.));
#9109=DIRECTION('center_axis',(0.,1.,0.));
#9110=DIRECTION('ref_axis',(1.,0.,0.));
#9111=DIRECTION('center_axis',(0.,1.,0.));
#9112=DIRECTION('ref_axis',(1.,0.,0.));
#9113=DIRECTION('center_axis',(0.,-1.,0.));
#9114=DIRECTION('ref_axis',(1.,0.,0.));
#9115=DIRECTION('center_axis',(0.,1.,0.));
#9116=DIRECTION('ref_axis',(1.,0.,0.));
#9117=DIRECTION('',(0.,-1.,0.));
#9118=DIRECTION('center_axis',(0.,1.,0.));
#9119=DIRECTION('ref_axis',(1.,0.,0.));
#9120=DIRECTION('center_axis',(0.,1.,0.));
#9121=DIRECTION('ref_axis',(1.,0.,0.));
#9122=DIRECTION('center_axis',(0.,1.,0.));
#9123=DIRECTION('ref_axis',(0.,0.,1.));
#9124=DIRECTION('center_axis',(0.,-1.,0.));
#9125=DIRECTION('ref_axis',(1.,0.,0.));
#9126=DIRECTION('center_axis',(0.,-1.,0.));
#9127=DIRECTION('ref_axis',(1.,0.,0.));
#9128=DIRECTION('center_axis',(0.,-1.,0.));
#9129=DIRECTION('ref_axis',(1.,0.,0.));
#9130=DIRECTION('',(0.707106781186547,0.707106781186548,8.65956056235493E-17));
#9131=DIRECTION('center_axis',(0.,-1.,0.));
#9132=DIRECTION('ref_axis',(1.,0.,0.));
#9133=DIRECTION('center_axis',(0.,-1.,0.));
#9134=DIRECTION('ref_axis',(1.,0.,0.));
#9135=DIRECTION('',(0.,1.,0.));
#9136=DIRECTION('center_axis',(0.,1.,0.));
#9137=DIRECTION('ref_axis',(1.,0.,0.));
#9138=DIRECTION('center_axis',(0.,-1.,0.));
#9139=DIRECTION('ref_axis',(1.,0.,0.));
#9140=DIRECTION('',(-0.707106781186547,0.707106781186548,-8.65956056235493E-17));
#9141=DIRECTION('center_axis',(0.,-1.,0.));
#9142=DIRECTION('ref_axis',(0.,0.,-1.));
#9143=DIRECTION('center_axis',(0.,-1.,0.));
#9144=DIRECTION('ref_axis',(1.,0.,0.));
#9145=DIRECTION('center_axis',(0.,1.,0.));
#9146=DIRECTION('ref_axis',(1.,0.,0.));
#9147=DIRECTION('center_axis',(0.,1.,0.));
#9148=DIRECTION('ref_axis',(1.,0.,0.));
#9149=DIRECTION('',(-0.447213595499958,0.894427190999916,-5.47678698264203E-17));
#9150=DIRECTION('center_axis',(0.,-1.,0.));
#9151=DIRECTION('ref_axis',(1.,0.,0.));
#9152=DIRECTION('center_axis',(0.,1.,0.));
#9153=DIRECTION('ref_axis',(1.,0.,0.));
#9154=DIRECTION('',(0.,1.,0.));
#9155=DIRECTION('center_axis',(0.,1.,0.));
#9156=DIRECTION('ref_axis',(1.,0.,0.));
#9157=DIRECTION('',(-0.707106781186547,0.707106781186548,-8.65956056235493E-17));
#9158=DIRECTION('axis',(0.,0.,1.));
#9159=DIRECTION('refdir',(1.,0.,0.));
#9160=DIRECTION('axis',(0.,0.,1.));
#9161=DIRECTION('refdir',(1.,0.,0.));
#9162=DIRECTION('center_axis',(0.,1.,0.));
#9163=DIRECTION('ref_axis',(1.,0.,0.));
#9164=DIRECTION('center_axis',(0.,1.,0.));
#9165=DIRECTION('ref_axis',(1.,0.,0.));
#9166=DIRECTION('',(0.,1.,0.));
#9167=DIRECTION('center_axis',(0.,-1.,0.));
#9168=DIRECTION('ref_axis',(1.,0.,0.));
#9169=DIRECTION('center_axis',(0.,1.,0.));
#9170=DIRECTION('ref_axis',(-0.46947156278589,0.,0.882947592858928));
#9171=DIRECTION('',(0.,-1.,0.));
#9172=DIRECTION('center_axis',(0.,1.,0.));
#9173=DIRECTION('ref_axis',(1.,0.,0.));
#9174=DIRECTION('',(0.,1.,0.));
#9175=DIRECTION('center_axis',(0.,1.,0.));
#9176=DIRECTION('ref_axis',(1.,0.,0.));
#9177=DIRECTION('center_axis',(0.,1.,0.));
#9178=DIRECTION('ref_axis',(1.,0.,0.));
#9179=DIRECTION('',(-0.469471562785891,0.,0.882947592858927));
#9180=DIRECTION('center_axis',(0.,1.,0.));
#9181=DIRECTION('ref_axis',(1.,0.,0.));
#9182=DIRECTION('center_axis',(0.,1.,0.));
#9183=DIRECTION('ref_axis',(1.,0.,0.));
#9184=DIRECTION('',(-0.469471562785891,0.,0.882947592858927));
#9185=DIRECTION('center_axis',(0.,1.,0.));
#9186=DIRECTION('ref_axis',(1.,0.,0.));
#9187=DIRECTION('',(0.469471562785891,0.,-0.882947592858927));
#9188=DIRECTION('center_axis',(0.,1.,0.));
#9189=DIRECTION('ref_axis',(1.,0.,0.));
#9190=DIRECTION('',(0.469471562785891,0.,-0.882947592858927));
#9191=DIRECTION('center_axis',(0.,-1.,0.));
#9192=DIRECTION('ref_axis',(1.,0.,0.));
#9193=DIRECTION('center_axis',(-0.882947592858927,0.,-0.469471562785891));
#9194=DIRECTION('ref_axis',(-0.469471562785891,0.,0.882947592858927));
#9195=DIRECTION('',(-0.469471562785891,0.,0.882947592858927));
#9196=DIRECTION('',(0.,1.,0.));
#9197=DIRECTION('center_axis',(0.,1.,0.));
#9198=DIRECTION('ref_axis',(0.,0.,1.));
#9199=DIRECTION('',(0.469471562785891,0.,-0.882947592858927));
#9200=DIRECTION('center_axis',(0.,1.,0.));
#9201=DIRECTION('ref_axis',(1.,0.,0.));
#9202=DIRECTION('center_axis',(0.882947592858927,0.,0.469471562785891));
#9203=DIRECTION('ref_axis',(0.469471562785891,0.,-0.882947592858927));
#9204=DIRECTION('',(0.,-1.,0.));
#9205=DIRECTION('center_axis',(0.,1.,0.));
#9206=DIRECTION('ref_axis',(0.46947156278589,0.,-0.882947592858927));
#9207=DIRECTION('',(0.,-1.,0.));
#9208=DIRECTION('center_axis',(0.,1.,0.));
#9209=DIRECTION('ref_axis',(1.,0.,0.));
#9210=DIRECTION('',(0.,1.,0.));
#9211=DIRECTION('center_axis',(0.882947592858927,0.,0.469471562785891));
#9212=DIRECTION('ref_axis',(0.469471562785891,0.,-0.882947592858927));
#9213=DIRECTION('',(0.469471562785891,0.,-0.882947592858927));
#9214=DIRECTION('',(0.,1.,0.));
#9215=DIRECTION('center_axis',(0.,1.,0.));
#9216=DIRECTION('ref_axis',(0.,0.,1.));
#9217=DIRECTION('',(-0.469471562785891,0.,0.882947592858927));
#9218=DIRECTION('center_axis',(0.,1.,0.));
#9219=DIRECTION('ref_axis',(1.,0.,0.));
#9220=DIRECTION('center_axis',(-0.882947592858927,0.,-0.469471562785891));
#9221=DIRECTION('ref_axis',(-0.469471562785891,0.,0.882947592858927));
#9222=DIRECTION('',(0.,-1.,0.));
#9223=DIRECTION('center_axis',(0.,1.,0.));
#9224=DIRECTION('ref_axis',(1.,0.,0.));
#9225=DIRECTION('center_axis',(0.,1.,0.));
#9226=DIRECTION('ref_axis',(1.,0.,0.));
#9227=DIRECTION('center_axis',(0.,1.,0.));
#9228=DIRECTION('ref_axis',(1.,0.,0.));
#9229=DIRECTION('center_axis',(0.,1.,0.));
#9230=DIRECTION('ref_axis',(1.,0.,0.));
#9231=DIRECTION('',(0.,-1.,0.));
#9232=DIRECTION('center_axis',(0.,1.,0.));
#9233=DIRECTION('ref_axis',(1.,0.,0.));
#9234=DIRECTION('center_axis',(0.,1.,0.));
#9235=DIRECTION('ref_axis',(1.,0.,0.));
#9236=DIRECTION('center_axis',(0.,1.,0.));
#9237=DIRECTION('ref_axis',(1.,0.,0.));
#9238=DIRECTION('center_axis',(0.,1.,0.));
#9239=DIRECTION('ref_axis',(1.,0.,0.));
#9240=DIRECTION('',(0.,-1.,0.));
#9241=DIRECTION('center_axis',(0.,1.,0.));
#9242=DIRECTION('ref_axis',(1.,0.,0.));
#9243=DIRECTION('',(0.,-1.,0.));
#9244=DIRECTION('center_axis',(0.,1.,0.));
#9245=DIRECTION('ref_axis',(1.,0.,0.));
#9246=DIRECTION('center_axis',(0.,1.,0.));
#9247=DIRECTION('ref_axis',(1.,0.,0.));
#9248=DIRECTION('center_axis',(0.,1.,0.));
#9249=DIRECTION('ref_axis',(1.,0.,0.));
#9250=DIRECTION('',(0.,-1.,0.));
#9251=DIRECTION('center_axis',(0.,1.,0.));
#9252=DIRECTION('ref_axis',(1.,0.,0.));
#9253=DIRECTION('center_axis',(0.,1.,0.));
#9254=DIRECTION('ref_axis',(1.,0.,0.));
#9255=DIRECTION('axis',(0.,0.,1.));
#9256=DIRECTION('refdir',(1.,0.,0.));
#9257=DIRECTION('center_axis',(0.,1.,0.));
#9258=DIRECTION('ref_axis',(1.,0.,0.));
#9259=DIRECTION('center_axis',(0.,-1.,0.));
#9260=DIRECTION('ref_axis',(1.,0.,0.));
#9261=DIRECTION('',(0.,-1.,0.));
#9262=DIRECTION('center_axis',(0.,-1.,0.));
#9263=DIRECTION('ref_axis',(1.,0.,0.));
#9264=DIRECTION('center_axis',(0.,1.,0.));
#9265=DIRECTION('ref_axis',(1.,0.,0.));
#9266=DIRECTION('center_axis',(0.,1.,0.));
#9267=DIRECTION('ref_axis',(1.,0.,0.));
#9268=DIRECTION('',(0.,-1.,0.));
#9269=DIRECTION('center_axis',(0.,1.,0.));
#9270=DIRECTION('ref_axis',(1.,0.,0.));
#9271=DIRECTION('center_axis',(0.,1.,0.));
#9272=DIRECTION('ref_axis',(1.,0.,0.));
#9273=DIRECTION('center_axis',(0.,1.,0.));
#9274=DIRECTION('ref_axis',(1.,0.,0.));
#9275=DIRECTION('axis',(0.,0.,1.));
#9276=DIRECTION('refdir',(1.,0.,0.));
#9277=DIRECTION('center_axis',(1.,0.,0.));
#9278=DIRECTION('ref_axis',(0.,0.,-1.));
#9279=DIRECTION('',(0.,1.,0.));
#9280=DIRECTION('center_axis',(1.,0.,0.));
#9281=DIRECTION('ref_axis',(0.,0.,-1.));
#9282=DIRECTION('center_axis',(1.,0.,0.));
#9283=DIRECTION('ref_axis',(0.,0.,-1.));
#9284=DIRECTION('center_axis',(1.,0.,0.));
#9285=DIRECTION('ref_axis',(0.,0.,-1.));
#9286=DIRECTION('',(1.,0.,0.));
#9287=DIRECTION('center_axis',(1.,0.,0.));
#9288=DIRECTION('ref_axis',(0.,0.,-1.));
#9289=DIRECTION('center_axis',(1.,0.,0.));
#9290=DIRECTION('ref_axis',(0.,0.,-1.));
#9291=DIRECTION('',(0.,-1.,0.));
#9292=DIRECTION('center_axis',(0.,1.,0.));
#9293=DIRECTION('ref_axis',(1.,0.,0.));
#9294=DIRECTION('center_axis',(0.,-1.,0.));
#9295=DIRECTION('ref_axis',(1.,0.,0.));
#9296=DIRECTION('',(0.,-1.,0.));
#9297=DIRECTION('center_axis',(0.,-1.,0.));
#9298=DIRECTION('ref_axis',(1.,0.,0.));
#9299=DIRECTION('center_axis',(0.,1.,0.));
#9300=DIRECTION('ref_axis',(1.,0.,0.));
#9301=DIRECTION('center_axis',(0.,1.,0.));
#9302=DIRECTION('ref_axis',(1.,0.,0.));
#9303=DIRECTION('',(0.,-1.,0.));
#9304=DIRECTION('center_axis',(0.,1.,0.));
#9305=DIRECTION('ref_axis',(1.,0.,0.));
#9306=DIRECTION('center_axis',(0.,1.,0.));
#9307=DIRECTION('ref_axis',(1.,0.,0.));
#9308=DIRECTION('center_axis',(0.,1.,0.));
#9309=DIRECTION('ref_axis',(1.,0.,0.));
#9310=DIRECTION('axis',(0.,0.,1.));
#9311=DIRECTION('refdir',(1.,0.,0.));
#9312=DIRECTION('center_axis',(0.,1.,0.));
#9313=DIRECTION('ref_axis',(1.,0.,0.));
#9314=DIRECTION('center_axis',(0.,1.,0.));
#9315=DIRECTION('ref_axis',(1.,0.,0.));
#9316=DIRECTION('',(0.,1.,0.));
#9317=DIRECTION('center_axis',(0.,-1.,0.));
#9318=DIRECTION('ref_axis',(1.,0.,0.));
#9319=DIRECTION('center_axis',(0.,1.,0.));
#9320=DIRECTION('ref_axis',(1.,0.,0.));
#9321=DIRECTION('center_axis',(0.,1.,0.));
#9322=DIRECTION('ref_axis',(1.,0.,0.));
#9323=DIRECTION('center_axis',(0.,1.,0.));
#9324=DIRECTION('ref_axis',(1.,0.,0.));
#9325=DIRECTION('',(0.,1.,0.));
#9326=DIRECTION('center_axis',(0.,1.,0.));
#9327=DIRECTION('ref_axis',(1.,0.,0.));
#9328=DIRECTION('center_axis',(0.,1.,0.));
#9329=DIRECTION('ref_axis',(1.,0.,0.));
#9330=DIRECTION('center_axis',(0.,1.,0.));
#9331=DIRECTION('ref_axis',(1.,0.,0.));
#9332=DIRECTION('center_axis',(0.,1.,0.));
#9333=DIRECTION('ref_axis',(1.,0.,0.));
#9334=DIRECTION('center_axis',(0.,1.,0.));
#9335=DIRECTION('ref_axis',(1.,0.,0.));
#9336=DIRECTION('center_axis',(0.,1.,0.));
#9337=DIRECTION('ref_axis',(1.,0.,0.));
#9338=DIRECTION('center_axis',(0.,1.,0.));
#9339=DIRECTION('ref_axis',(1.,0.,0.));
#9340=DIRECTION('center_axis',(0.,-1.,0.));
#9341=DIRECTION('ref_axis',(1.,0.,0.));
#9342=DIRECTION('center_axis',(0.,1.,0.));
#9343=DIRECTION('ref_axis',(1.,0.,0.));
#9344=DIRECTION('',(0.,-1.,0.));
#9345=DIRECTION('center_axis',(0.,1.,0.));
#9346=DIRECTION('ref_axis',(1.,0.,0.));
#9347=DIRECTION('',(0.,-1.,0.));
#9348=DIRECTION('center_axis',(0.,1.,0.));
#9349=DIRECTION('ref_axis',(1.,0.,0.));
#9350=DIRECTION('center_axis',(0.,1.,0.));
#9351=DIRECTION('ref_axis',(1.,0.,0.));
#9352=DIRECTION('center_axis',(0.,1.,0.));
#9353=DIRECTION('ref_axis',(1.,0.,0.));
#9354=DIRECTION('',(0.,-1.,0.));
#9355=DIRECTION('center_axis',(0.,1.,0.));
#9356=DIRECTION('ref_axis',(1.,0.,0.));
#9357=DIRECTION('center_axis',(0.,1.,0.));
#9358=DIRECTION('ref_axis',(1.,0.,0.));
#9359=DIRECTION('axis',(0.,0.,1.));
#9360=DIRECTION('refdir',(1.,0.,0.));
#9361=DIRECTION('center_axis',(0.,1.,0.));
#9362=DIRECTION('ref_axis',(1.,0.,0.));
#9363=DIRECTION('center_axis',(0.,-1.,0.));
#9364=DIRECTION('ref_axis',(1.,0.,0.));
#9365=DIRECTION('',(0.,-1.,0.));
#9366=DIRECTION('center_axis',(0.,-1.,0.));
#9367=DIRECTION('ref_axis',(1.,0.,0.));
#9368=DIRECTION('center_axis',(0.,1.,0.));
#9369=DIRECTION('ref_axis',(1.,0.,0.));
#9370=DIRECTION('center_axis',(0.,1.,0.));
#9371=DIRECTION('ref_axis',(1.,0.,0.));
#9372=DIRECTION('',(0.,-1.,0.));
#9373=DIRECTION('center_axis',(0.,1.,0.));
#9374=DIRECTION('ref_axis',(1.,0.,0.));
#9375=DIRECTION('center_axis',(0.,1.,0.));
#9376=DIRECTION('ref_axis',(1.,0.,0.));
#9377=DIRECTION('center_axis',(0.,1.,0.));
#9378=DIRECTION('ref_axis',(1.,0.,0.));
#9379=DIRECTION('axis',(0.,0.,1.));
#9380=DIRECTION('refdir',(1.,0.,0.));
#9381=DIRECTION('center_axis',(0.,1.,0.));
#9382=DIRECTION('ref_axis',(1.,0.,0.));
#9383=DIRECTION('center_axis',(0.,-1.,0.));
#9384=DIRECTION('ref_axis',(1.,0.,0.));
#9385=DIRECTION('',(0.,-1.,0.));
#9386=DIRECTION('center_axis',(0.,-1.,0.));
#9387=DIRECTION('ref_axis',(1.,0.,0.));
#9388=DIRECTION('center_axis',(0.,1.,0.));
#9389=DIRECTION('ref_axis',(1.,0.,0.));
#9390=DIRECTION('center_axis',(0.,1.,0.));
#9391=DIRECTION('ref_axis',(1.,0.,0.));
#9392=DIRECTION('',(0.,-1.,0.));
#9393=DIRECTION('center_axis',(0.,1.,0.));
#9394=DIRECTION('ref_axis',(1.,0.,0.));
#9395=DIRECTION('center_axis',(0.,1.,0.));
#9396=DIRECTION('ref_axis',(1.,0.,0.));
#9397=DIRECTION('center_axis',(0.,1.,0.));
#9398=DIRECTION('ref_axis',(1.,0.,0.));
#9399=DIRECTION('axis',(0.,0.,1.));
#9400=DIRECTION('refdir',(1.,0.,0.));
#9401=DIRECTION('center_axis',(0.,1.,0.));
#9402=DIRECTION('ref_axis',(1.,0.,0.));
#9403=DIRECTION('center_axis',(0.,-1.,0.));
#9404=DIRECTION('ref_axis',(1.,0.,0.));
#9405=DIRECTION('',(0.,-1.,0.));
#9406=DIRECTION('center_axis',(0.,-1.,0.));
#9407=DIRECTION('ref_axis',(1.,0.,0.));
#9408=DIRECTION('center_axis',(0.,1.,0.));
#9409=DIRECTION('ref_axis',(1.,0.,0.));
#9410=DIRECTION('center_axis',(0.,1.,0.));
#9411=DIRECTION('ref_axis',(1.,0.,0.));
#9412=DIRECTION('',(0.,-1.,0.));
#9413=DIRECTION('center_axis',(0.,1.,0.));
#9414=DIRECTION('ref_axis',(1.,0.,0.));
#9415=DIRECTION('center_axis',(0.,1.,0.));
#9416=DIRECTION('ref_axis',(1.,0.,0.));
#9417=DIRECTION('center_axis',(0.,1.,0.));
#9418=DIRECTION('ref_axis',(1.,0.,0.));
#9419=DIRECTION('axis',(0.,0.,1.));
#9420=DIRECTION('refdir',(1.,0.,0.));
#9421=DIRECTION('center_axis',(0.,1.,0.));
#9422=DIRECTION('ref_axis',(1.,0.,0.));
#9423=DIRECTION('center_axis',(0.,-1.,0.));
#9424=DIRECTION('ref_axis',(1.,0.,0.));
#9425=DIRECTION('',(0.,-1.,0.));
#9426=DIRECTION('center_axis',(0.,-1.,0.));
#9427=DIRECTION('ref_axis',(1.,0.,0.));
#9428=DIRECTION('center_axis',(0.,1.,0.));
#9429=DIRECTION('ref_axis',(1.,0.,0.));
#9430=DIRECTION('center_axis',(0.,1.,0.));
#9431=DIRECTION('ref_axis',(1.,0.,0.));
#9432=DIRECTION('',(0.,-1.,0.));
#9433=DIRECTION('center_axis',(0.,1.,0.));
#9434=DIRECTION('ref_axis',(1.,0.,0.));
#9435=DIRECTION('center_axis',(0.,1.,0.));
#9436=DIRECTION('ref_axis',(1.,0.,0.));
#9437=DIRECTION('center_axis',(0.,1.,0.));
#9438=DIRECTION('ref_axis',(1.,0.,0.));
#9439=DIRECTION('axis',(0.,0.,1.));
#9440=DIRECTION('refdir',(1.,0.,0.));
#9441=DIRECTION('center_axis',(0.,1.,0.));
#9442=DIRECTION('ref_axis',(1.,0.,0.));
#9443=DIRECTION('center_axis',(0.,1.,0.));
#9444=DIRECTION('ref_axis',(1.,0.,0.));
#9445=DIRECTION('center_axis',(0.866025403784439,0.,-0.5));
#9446=DIRECTION('ref_axis',(0.5,0.,0.866025403784439));
#9447=DIRECTION('',(0.5,0.,0.866025403784439));
#9448=DIRECTION('',(0.,-1.,0.));
#9449=DIRECTION('',(0.5,0.,0.866025403784439));
#9450=DIRECTION('',(0.,-1.,0.));
#9451=DIRECTION('center_axis',(1.20185167898973E-16,0.,-1.));
#9452=DIRECTION('ref_axis',(1.,0.,1.20185167898973E-16));
#9453=DIRECTION('',(1.,0.,1.20185167898973E-16));
#9454=DIRECTION('',(0.,-1.,0.));
#9455=DIRECTION('',(1.,0.,1.20185167898973E-16));
#9456=DIRECTION('center_axis',(-0.866025403784439,0.,-0.5));
#9457=DIRECTION('ref_axis',(0.5,0.,-0.866025403784439));
#9458=DIRECTION('',(0.5,0.,-0.866025403784439));
#9459=DIRECTION('',(0.,-1.,0.));
#9460=DIRECTION('',(0.5,0.,-0.866025403784439));
#9461=DIRECTION('center_axis',(-0.866025403784439,0.,0.5));
#9462=DIRECTION('ref_axis',(-0.5,0.,-0.866025403784439));
#9463=DIRECTION('',(-0.5,0.,-0.866025403784439));
#9464=DIRECTION('',(0.,-1.,0.));
#9465=DIRECTION('',(-0.5,0.,-0.866025403784439));
#9466=DIRECTION('center_axis',(-2.40370335797945E-16,0.,1.));
#9467=DIRECTION('ref_axis',(-1.,0.,-2.40370335797945E-16));
#9468=DIRECTION('',(-1.,0.,-2.40370335797945E-16));
#9469=DIRECTION('',(0.,-1.,0.));
#9470=DIRECTION('',(-1.,0.,-2.40370335797945E-16));
#9471=DIRECTION('center_axis',(0.866025403784439,0.,0.5));
#9472=DIRECTION('ref_axis',(-0.5,0.,0.866025403784439));
#9473=DIRECTION('',(-0.5,0.,0.866025403784439));
#9474=DIRECTION('',(-0.5,0.,0.866025403784439));
#9475=DIRECTION('center_axis',(0.,-1.,0.));
#9476=DIRECTION('ref_axis',(0.,0.,-1.));
#9477=DIRECTION('center_axis',(0.,1.,0.));
#9478=DIRECTION('ref_axis',(0.,0.,1.));
#9479=DIRECTION('center_axis',(0.,-1.,0.));
#9480=DIRECTION('ref_axis',(1.,0.,0.));
#9481=DIRECTION('center_axis',(0.,-1.,0.));
#9482=DIRECTION('ref_axis',(1.,0.,0.));
#9483=DIRECTION('center_axis',(0.,-1.,0.));
#9484=DIRECTION('ref_axis',(1.,0.,0.));
#9485=DIRECTION('',(0.707106781186548,0.707106781186547,8.65956056235494E-17));
#9486=DIRECTION('center_axis',(0.,-1.,0.));
#9487=DIRECTION('ref_axis',(1.,0.,0.));
#9488=DIRECTION('',(0.,1.,0.));
#9489=DIRECTION('axis',(0.,0.,1.));
#9490=DIRECTION('refdir',(1.,0.,0.));
#9491=DIRECTION('center_axis',(0.866025403784439,0.,-0.5));
#9492=DIRECTION('ref_axis',(0.5,0.,0.866025403784439));
#9493=DIRECTION('',(-0.5,0.,-0.866025403784439));
#9494=DIRECTION('',(0.,-1.,0.));
#9495=DIRECTION('',(0.5,0.,0.866025403784439));
#9496=DIRECTION('',(0.,-1.,0.));
#9497=DIRECTION('center_axis',(1.60246890531964E-16,0.,-1.));
#9498=DIRECTION('ref_axis',(1.,0.,1.60246890531964E-16));
#9499=DIRECTION('',(-1.,0.,-1.60246890531964E-16));
#9500=DIRECTION('',(0.,-1.,0.));
#9501=DIRECTION('',(1.,0.,1.60246890531964E-16));
#9502=DIRECTION('center_axis',(-0.866025403784439,0.,-0.5));
#9503=DIRECTION('ref_axis',(0.5,0.,-0.866025403784439));
#9504=DIRECTION('',(-0.5,0.,0.866025403784439));
#9505=DIRECTION('',(0.,-1.,0.));
#9506=DIRECTION('',(0.5,0.,-0.866025403784439));
#9507=DIRECTION('center_axis',(-0.866025403784439,0.,0.5));
#9508=DIRECTION('ref_axis',(-0.5,0.,-0.866025403784439));
#9509=DIRECTION('',(0.5,0.,0.866025403784439));
#9510=DIRECTION('',(0.,-1.,0.));
#9511=DIRECTION('',(-0.5,0.,-0.866025403784439));
#9512=DIRECTION('center_axis',(-1.60246890531964E-16,0.,1.));
#9513=DIRECTION('ref_axis',(-1.,0.,-1.60246890531964E-16));
#9514=DIRECTION('',(1.,0.,1.60246890531964E-16));
#9515=DIRECTION('',(0.,-1.,0.));
#9516=DIRECTION('',(-1.,0.,-1.60246890531964E-16));
#9517=DIRECTION('center_axis',(0.866025403784439,0.,0.5));
#9518=DIRECTION('ref_axis',(-0.5,0.,0.866025403784439));
#9519=DIRECTION('',(0.5,0.,-0.866025403784439));
#9520=DIRECTION('',(-0.5,0.,0.866025403784439));
#9521=DIRECTION('center_axis',(0.,1.,0.));
#9522=DIRECTION('ref_axis',(1.,0.,0.));
#9523=DIRECTION('center_axis',(0.,-1.,0.));
#9524=DIRECTION('ref_axis',(0.,0.,-1.));
#9525=DIRECTION('center_axis',(0.,1.,0.));
#9526=DIRECTION('ref_axis',(1.,0.,0.));
#9527=DIRECTION('center_axis',(0.,1.,0.));
#9528=DIRECTION('ref_axis',(1.,0.,0.));
#9529=DIRECTION('center_axis',(0.,1.,0.));
#9530=DIRECTION('ref_axis',(0.,0.,1.));
#9531=DIRECTION('center_axis',(0.,-1.,0.));
#9532=DIRECTION('ref_axis',(1.,0.,0.));
#9533=DIRECTION('center_axis',(0.,-1.,0.));
#9534=DIRECTION('ref_axis',(1.,0.,0.));
#9535=DIRECTION('center_axis',(0.,-1.,0.));
#9536=DIRECTION('ref_axis',(1.,0.,0.));
#9537=DIRECTION('',(0.707106781186547,0.707106781186548,8.65956056235493E-17));
#9538=DIRECTION('center_axis',(0.,-1.,0.));
#9539=DIRECTION('ref_axis',(1.,0.,0.));
#9540=DIRECTION('center_axis',(0.,-1.,0.));
#9541=DIRECTION('ref_axis',(1.,0.,0.));
#9542=DIRECTION('',(0.,1.,0.));
#9543=DIRECTION('center_axis',(0.,1.,0.));
#9544=DIRECTION('ref_axis',(1.,0.,0.));
#9545=DIRECTION('center_axis',(0.,-1.,0.));
#9546=DIRECTION('ref_axis',(1.,0.,0.));
#9547=DIRECTION('',(-0.707106781186547,0.707106781186548,-8.65956056235493E-17));
#9548=DIRECTION('center_axis',(0.,-1.,0.));
#9549=DIRECTION('ref_axis',(0.,0.,-1.));
#9550=DIRECTION('center_axis',(0.,-1.,0.));
#9551=DIRECTION('ref_axis',(1.,0.,0.));
#9552=DIRECTION('center_axis',(0.,1.,0.));
#9553=DIRECTION('ref_axis',(1.,0.,0.));
#9554=DIRECTION('center_axis',(0.,1.,0.));
#9555=DIRECTION('ref_axis',(1.,0.,0.));
#9556=DIRECTION('',(-0.447213595499958,0.894427190999916,-5.47678698264203E-17));
#9557=DIRECTION('center_axis',(0.,-1.,0.));
#9558=DIRECTION('ref_axis',(1.,0.,0.));
#9559=DIRECTION('',(0.,1.,0.));
#9560=DIRECTION('axis',(0.,0.,1.));
#9561=DIRECTION('refdir',(1.,0.,0.));
#9562=DIRECTION('center_axis',(0.,1.,0.));
#9563=DIRECTION('ref_axis',(0.,0.,1.));
#9564=DIRECTION('center_axis',(0.,-1.,0.));
#9565=DIRECTION('ref_axis',(1.,0.,0.));
#9566=DIRECTION('center_axis',(0.,-1.,0.));
#9567=DIRECTION('ref_axis',(1.,0.,0.));
#9568=DIRECTION('center_axis',(0.,-1.,0.));
#9569=DIRECTION('ref_axis',(1.,0.,0.));
#9570=DIRECTION('',(0.707106781186547,0.707106781186548,8.65956056235493E-17));
#9571=DIRECTION('center_axis',(0.,-1.,0.));
#9572=DIRECTION('ref_axis',(1.,0.,0.));
#9573=DIRECTION('center_axis',(0.,-1.,0.));
#9574=DIRECTION('ref_axis',(1.,0.,0.));
#9575=DIRECTION('',(0.,1.,0.));
#9576=DIRECTION('center_axis',(0.,1.,0.));
#9577=DIRECTION('ref_axis',(1.,0.,0.));
#9578=DIRECTION('center_axis',(0.,-1.,0.));
#9579=DIRECTION('ref_axis',(1.,0.,0.));
#9580=DIRECTION('',(-0.707106781186547,0.707106781186548,-8.65956056235493E-17));
#9581=DIRECTION('center_axis',(0.,-1.,0.));
#9582=DIRECTION('ref_axis',(0.,0.,-1.));
#9583=DIRECTION('center_axis',(0.,-1.,0.));
#9584=DIRECTION('ref_axis',(1.,0.,0.));
#9585=DIRECTION('center_axis',(0.,1.,0.));
#9586=DIRECTION('ref_axis',(1.,0.,0.));
#9587=DIRECTION('center_axis',(0.,1.,0.));
#9588=DIRECTION('ref_axis',(1.,0.,0.));
#9589=DIRECTION('',(-0.447213595499958,0.894427190999916,-5.47678698264203E-17));
#9590=DIRECTION('center_axis',(0.,-1.,0.));
#9591=DIRECTION('ref_axis',(1.,0.,0.));
#9592=DIRECTION('center_axis',(0.,1.,0.));
#9593=DIRECTION('ref_axis',(1.,0.,0.));
#9594=DIRECTION('',(0.,1.,0.));
#9595=DIRECTION('center_axis',(0.,1.,0.));
#9596=DIRECTION('ref_axis',(1.,0.,0.));
#9597=DIRECTION('center_axis',(0.,-1.,0.));
#9598=DIRECTION('ref_axis',(1.,0.,0.));
#9599=DIRECTION('',(-0.707106781186547,0.707106781186548,-8.65956056235493E-17));
#9600=DIRECTION('center_axis',(0.,-1.,0.));
#9601=DIRECTION('ref_axis',(0.,0.,-1.));
#9602=DIRECTION('center_axis',(0.866025403784439,0.,-0.5));
#9603=DIRECTION('ref_axis',(0.5,0.,0.866025403784439));
#9604=DIRECTION('',(-0.5,0.,-0.866025403784439));
#9605=DIRECTION('',(0.,-1.,0.));
#9606=DIRECTION('',(0.5,0.,0.866025403784439));
#9607=DIRECTION('',(0.,-1.,0.));
#9608=DIRECTION('center_axis',(1.60246890531964E-16,0.,-1.));
#9609=DIRECTION('ref_axis',(1.,0.,1.60246890531964E-16));
#9610=DIRECTION('',(-1.,0.,-1.60246890531964E-16));
#9611=DIRECTION('',(0.,-1.,0.));
#9612=DIRECTION('',(1.,0.,1.60246890531964E-16));
#9613=DIRECTION('center_axis',(-0.866025403784439,0.,-0.5));
#9614=DIRECTION('ref_axis',(0.5,0.,-0.866025403784439));
#9615=DIRECTION('',(-0.5,0.,0.866025403784439));
#9616=DIRECTION('',(0.,-1.,0.));
#9617=DIRECTION('',(0.5,0.,-0.866025403784439));
#9618=DIRECTION('center_axis',(-0.866025403784439,0.,0.5));
#9619=DIRECTION('ref_axis',(-0.5,0.,-0.866025403784439));
#9620=DIRECTION('',(0.5,0.,0.866025403784439));
#9621=DIRECTION('',(0.,-1.,0.));
#9622=DIRECTION('',(-0.5,0.,-0.866025403784439));
#9623=DIRECTION('center_axis',(-1.60246890531964E-16,0.,1.));
#9624=DIRECTION('ref_axis',(-1.,0.,-1.60246890531964E-16));
#9625=DIRECTION('',(1.,0.,1.60246890531964E-16));
#9626=DIRECTION('',(0.,-1.,0.));
#9627=DIRECTION('',(-1.,0.,-1.60246890531964E-16));
#9628=DIRECTION('center_axis',(0.866025403784439,0.,0.5));
#9629=DIRECTION('ref_axis',(-0.5,0.,0.866025403784439));
#9630=DIRECTION('',(0.5,0.,-0.866025403784439));
#9631=DIRECTION('',(-0.5,0.,0.866025403784439));
#9632=DIRECTION('center_axis',(0.,1.,0.));
#9633=DIRECTION('ref_axis',(1.,0.,0.));
#9634=DIRECTION('center_axis',(0.,-1.,0.));
#9635=DIRECTION('ref_axis',(0.,0.,-1.));
#9636=DIRECTION('',(0.,0.,1.));
#9637=DIRECTION('',(1.,0.,0.));
#9638=DIRECTION('',(0.,0.,1.));
#9639=DIRECTION('',(1.,0.,0.));
#9640=DIRECTION('',(0.,0.,1.));
#9641=DIRECTION('',(1.,0.,0.));
#9642=DIRECTION('',(0.,0.,1.));
#9643=DIRECTION('',(1.,0.,0.));
#9644=DIRECTION('',(0.,0.,1.));
#9645=DIRECTION('',(1.,0.,0.));
#9646=DIRECTION('',(0.,0.,1.));
#9647=DIRECTION('',(1.,0.,0.));
#9648=DIRECTION('',(0.,0.,1.));
#9649=DIRECTION('',(1.,0.,0.));
#9650=DIRECTION('',(0.,0.,1.));
#9651=DIRECTION('',(1.,0.,0.));
#9652=DIRECTION('',(0.,0.,1.));
#9653=DIRECTION('',(1.,0.,0.));
#9654=DIRECTION('',(0.,0.,1.));
#9655=DIRECTION('',(1.,0.,0.));
#9656=DIRECTION('',(0.,0.,1.));
#9657=DIRECTION('',(1.,0.,0.));
#9658=DIRECTION('',(0.,-1.,2.22044604925031E-16));
#9659=DIRECTION('',(1.,0.,0.));
#9660=DIRECTION('',(0.,-1.,2.22044604925031E-16));
#9661=DIRECTION('',(1.,0.,0.));
#9662=DIRECTION('',(0.,-1.,2.22044604925031E-16));
#9663=DIRECTION('',(1.,0.,0.));
#9664=DIRECTION('',(0.,-1.,2.22044604925031E-16));
#9665=DIRECTION('',(1.,0.,0.));
#9666=DIRECTION('',(0.,0.,1.));
#9667=DIRECTION('',(1.,0.,0.));
#9668=DIRECTION('',(0.,-1.,2.22044604925031E-16));
#9669=DIRECTION('',(1.,0.,0.));
#9670=DIRECTION('',(0.,0.,1.));
#9671=DIRECTION('',(-1.,1.22464679914735E-16,0.));
#9672=DIRECTION('',(0.,0.,1.));
#9673=DIRECTION('',(-1.,1.22464679914735E-16,0.));
#9674=DIRECTION('',(0.,0.,1.));
#9675=DIRECTION('',(-1.,1.22464679914735E-16,0.));
#9676=DIRECTION('',(0.,0.,1.));
#9677=DIRECTION('',(-1.,1.22464679914735E-16,0.));
#9678=DIRECTION('',(0.,0.,1.));
#9679=DIRECTION('',(1.,0.,0.));
#9680=DIRECTION('',(0.,0.,1.));
#9681=DIRECTION('',(1.,0.,0.));
#9682=DIRECTION('',(0.,0.,1.));
#9683=DIRECTION('',(1.,0.,0.));
#9684=DIRECTION('',(0.,0.,1.));
#9685=DIRECTION('',(1.,0.,0.));
#9686=DIRECTION('',(0.,-1.,2.22044604925031E-16));
#9687=DIRECTION('',(1.,0.,0.));
#9688=DIRECTION('',(0.,-1.,2.22044604925031E-16));
#9689=DIRECTION('',(1.,0.,0.));
#9690=DIRECTION('',(0.,-1.,2.22044604925031E-16));
#9691=DIRECTION('',(1.,0.,0.));
#9692=DIRECTION('',(0.,-1.,2.22044604925031E-16));
#9693=DIRECTION('',(1.,0.,0.));
#9694=DIRECTION('',(0.,1.,2.22044604925031E-16));
#9695=DIRECTION('',(1.,0.,0.));
#9696=DIRECTION('',(0.,1.,2.22044604925031E-16));
#9697=DIRECTION('',(1.,0.,0.));
#9698=DIRECTION('',(0.,1.,2.22044604925031E-16));
#9699=DIRECTION('',(1.,0.,0.));
#9700=DIRECTION('',(0.,1.,2.22044604925031E-16));
#9701=DIRECTION('',(1.,0.,0.));
#9702=DIRECTION('',(0.,0.,1.));
#9703=DIRECTION('',(1.,0.,0.));
#9704=DIRECTION('',(0.,0.,1.));
#9705=DIRECTION('',(1.,0.,0.));
#9706=DIRECTION('',(0.,0.,1.));
#9707=DIRECTION('',(1.,0.,0.));
#9708=DIRECTION('',(0.,0.,1.));
#9709=DIRECTION('',(1.,0.,0.));
#9710=DIRECTION('',(0.,0.,1.));
#9711=DIRECTION('',(1.,0.,0.));
#9712=DIRECTION('',(0.,0.,1.));
#9713=DIRECTION('',(1.,0.,0.));
#9714=DIRECTION('',(0.,0.,1.));
#9715=DIRECTION('',(1.,0.,0.));
#9716=DIRECTION('',(0.,0.,1.));
#9717=DIRECTION('',(1.,0.,0.));
#9718=DIRECTION('',(0.,0.,1.));
#9719=DIRECTION('',(1.,0.,0.));
#9720=DIRECTION('',(0.,0.,1.));
#9721=DIRECTION('',(2.22044604925031E-16,-1.,0.));
#9722=DIRECTION('',(0.,0.,1.));
#9723=DIRECTION('',(-1.,1.22464679914735E-16,0.));
#9724=DIRECTION('',(0.,0.,1.));
#9725=DIRECTION('',(1.,0.,0.));
#9726=DIRECTION('axis',(0.,0.,1.));
#9727=DIRECTION('refdir',(1.,0.,0.));
#9728=DIRECTION('axis',(0.,0.,1.));
#9729=DIRECTION('refdir',(1.,0.,0.));
#9730=DIRECTION('center_axis',(0.,1.,0.));
#9731=DIRECTION('ref_axis',(1.,0.,0.));
#9732=DIRECTION('center_axis',(0.,1.,0.));
#9733=DIRECTION('ref_axis',(1.,0.,0.));
#9734=DIRECTION('',(0.,1.,0.));
#9735=DIRECTION('center_axis',(0.,-1.,0.));
#9736=DIRECTION('ref_axis',(1.,0.,0.));
#9737=DIRECTION('center_axis',(0.,1.,0.));
#9738=DIRECTION('ref_axis',(1.,0.,0.));
#9739=DIRECTION('center_axis',(0.,1.,0.));
#9740=DIRECTION('ref_axis',(1.,0.,0.));
#9741=DIRECTION('',(0.,1.,0.));
#9742=DIRECTION('center_axis',(0.,-1.,0.));
#9743=DIRECTION('ref_axis',(1.,0.,0.));
#9744=DIRECTION('center_axis',(0.,1.,0.));
#9745=DIRECTION('ref_axis',(0.565264218607056,0.,-0.824909912149536));
#9746=DIRECTION('',(0.,-1.,0.));
#9747=DIRECTION('center_axis',(0.,1.,0.));
#9748=DIRECTION('ref_axis',(1.,0.,0.));
#9749=DIRECTION('',(0.,1.,0.));
#9750=DIRECTION('center_axis',(0.,1.,0.));
#9751=DIRECTION('ref_axis',(1.,0.,0.));
#9752=DIRECTION('center_axis',(-0.824909912149536,0.,-0.565264218607055));
#9753=DIRECTION('ref_axis',(-0.565264218607055,0.,0.824909912149537));
#9754=DIRECTION('',(-0.565264218607055,0.,0.824909912149537));
#9755=DIRECTION('',(0.,-1.,0.));
#9756=DIRECTION('',(-0.565264218607055,0.,0.824909912149537));
#9757=DIRECTION('center_axis',(0.,1.,0.));
#9758=DIRECTION('ref_axis',(1.,0.,0.));
#9759=DIRECTION('',(0.565264218607055,0.,-0.824909912149537));
#9760=DIRECTION('center_axis',(0.,1.,0.));
#9761=DIRECTION('ref_axis',(1.,0.,0.));
#9762=DIRECTION('center_axis',(0.824909912149536,0.,0.565264218607055));
#9763=DIRECTION('ref_axis',(0.565264218607055,0.,-0.824909912149537));
#9764=DIRECTION('',(0.565264218607055,0.,-0.824909912149537));
#9765=DIRECTION('',(0.,1.,0.));
#9766=DIRECTION('center_axis',(0.,1.,0.));
#9767=DIRECTION('ref_axis',(-0.565264218607055,0.,0.824909912149536));
#9768=DIRECTION('center_axis',(0.,1.,0.));
#9769=DIRECTION('ref_axis',(1.,0.,0.));
#9770=DIRECTION('center_axis',(0.,1.,0.));
#9771=DIRECTION('ref_axis',(1.,0.,0.));
#9772=DIRECTION('axis',(0.,0.,1.));
#9773=DIRECTION('refdir',(1.,0.,0.));
#9774=DIRECTION('center_axis',(0.,1.,0.));
#9775=DIRECTION('ref_axis',(1.,0.,0.));
#9776=DIRECTION('center_axis',(0.,-1.,0.));
#9777=DIRECTION('ref_axis',(1.,0.,0.));
#9778=DIRECTION('',(0.,-1.,0.));
#9779=DIRECTION('center_axis',(0.,-1.,0.));
#9780=DIRECTION('ref_axis',(1.,0.,0.));
#9781=DIRECTION('center_axis',(0.,1.,0.));
#9782=DIRECTION('ref_axis',(1.,0.,0.));
#9783=DIRECTION('center_axis',(0.,1.,0.));
#9784=DIRECTION('ref_axis',(1.,0.,0.));
#9785=DIRECTION('',(0.,-1.,0.));
#9786=DIRECTION('center_axis',(0.,1.,0.));
#9787=DIRECTION('ref_axis',(1.,0.,0.));
#9788=DIRECTION('center_axis',(0.,1.,0.));
#9789=DIRECTION('ref_axis',(1.,0.,0.));
#9790=DIRECTION('center_axis',(0.,1.,0.));
#9791=DIRECTION('ref_axis',(1.,0.,0.));
#9792=DIRECTION('axis',(0.,0.,1.));
#9793=DIRECTION('refdir',(1.,0.,0.));
#9794=DIRECTION('center_axis',(0.,1.,0.));
#9795=DIRECTION('ref_axis',(1.,0.,0.));
#9796=DIRECTION('center_axis',(0.,-1.,0.));
#9797=DIRECTION('ref_axis',(1.,0.,0.));
#9798=DIRECTION('',(0.,-1.,0.));
#9799=DIRECTION('center_axis',(0.,-1.,0.));
#9800=DIRECTION('ref_axis',(1.,0.,0.));
#9801=DIRECTION('center_axis',(0.,1.,0.));
#9802=DIRECTION('ref_axis',(1.,0.,0.));
#9803=DIRECTION('center_axis',(0.,1.,0.));
#9804=DIRECTION('ref_axis',(1.,0.,0.));
#9805=DIRECTION('',(0.,-1.,0.));
#9806=DIRECTION('center_axis',(0.,1.,0.));
#9807=DIRECTION('ref_axis',(1.,0.,0.));
#9808=DIRECTION('center_axis',(0.,1.,0.));
#9809=DIRECTION('ref_axis',(1.,0.,0.));
#9810=DIRECTION('center_axis',(0.,1.,0.));
#9811=DIRECTION('ref_axis',(1.,0.,0.));
#9812=DIRECTION('',(0.,0.,1.));
#9813=DIRECTION('',(1.,0.,0.));
#9814=DIRECTION('',(0.,0.,1.));
#9815=DIRECTION('',(1.,0.,0.));
#9816=DIRECTION('',(0.,0.,1.));
#9817=DIRECTION('',(1.,0.,0.));
#9818=DIRECTION('axis',(0.,0.,1.));
#9819=DIRECTION('refdir',(1.,0.,0.));
#9820=DIRECTION('axis',(0.,0.,1.));
#9821=DIRECTION('refdir',(1.,0.,0.));
#9822=DIRECTION('center_axis',(0.,1.,0.));
#9823=DIRECTION('ref_axis',(1.,0.,0.));
#9824=DIRECTION('center_axis',(0.,1.,0.));
#9825=DIRECTION('ref_axis',(1.,0.,0.));
#9826=DIRECTION('',(0.,1.,0.));
#9827=DIRECTION('center_axis',(0.,1.,0.));
#9828=DIRECTION('ref_axis',(1.,0.,0.));
#9829=DIRECTION('center_axis',(0.,1.,0.));
#9830=DIRECTION('ref_axis',(1.,0.,0.));
#9831=DIRECTION('center_axis',(0.,1.,0.));
#9832=DIRECTION('ref_axis',(0.,0.,1.));
#9833=DIRECTION('',(0.,0.,1.));
#9834=DIRECTION('',(-1.,0.,0.));
#9835=DIRECTION('',(0.,0.,-1.));
#9836=DIRECTION('',(1.,0.,0.));
#9837=DIRECTION('center_axis',(1.,0.,0.));
#9838=DIRECTION('ref_axis',(0.,1.,0.));
#9839=DIRECTION('',(0.,1.,0.));
#9840=DIRECTION('',(0.,0.,-1.));
#9841=DIRECTION('',(0.,-1.,0.));
#9842=DIRECTION('',(0.,0.,1.));
#9843=DIRECTION('',(0.,1.,0.));
#9844=DIRECTION('center_axis',(0.,0.,1.));
#9845=DIRECTION('ref_axis',(1.,0.,0.));
#9846=DIRECTION('',(0.,-1.,0.));
#9847=DIRECTION('center_axis',(0.,0.,-1.));
#9848=DIRECTION('ref_axis',(1.,0.,0.));
#9849=DIRECTION('center_axis',(-1.,0.,0.));
#9850=DIRECTION('ref_axis',(0.,-1.,0.));
#9851=DIRECTION('',(0.,-1.,0.));
#9852=DIRECTION('',(0.,0.,1.));
#9853=DIRECTION('',(0.,1.,0.));
#9854=DIRECTION('',(0.,0.,1.));
#9855=DIRECTION('center_axis',(0.,1.,0.));
#9856=DIRECTION('ref_axis',(-1.,0.,0.));
#9857=DIRECTION('',(0.,0.,-1.));
#9858=DIRECTION('',(-1.,0.,0.));
#9859=DIRECTION('',(1.,0.,0.));
#9860=DIRECTION('center_axis',(0.,1.,0.));
#9861=DIRECTION('ref_axis',(-1.,0.,0.));
#9862=DIRECTION('',(1.,0.,0.));
#9863=DIRECTION('',(-1.,0.,0.));
#9864=DIRECTION('',(0.,0.,1.));
#9865=DIRECTION('center_axis',(0.,0.,1.));
#9866=DIRECTION('ref_axis',(1.,0.,0.));
#9867=DIRECTION('center_axis',(0.,0.,1.));
#9868=DIRECTION('ref_axis',(1.,0.,0.));
#9869=DIRECTION('center_axis',(0.,0.,1.));
#9870=DIRECTION('ref_axis',(1.,0.,0.));
#9871=DIRECTION('center_axis',(0.,0.,1.));
#9872=DIRECTION('ref_axis',(1.,0.,0.));
#9873=DIRECTION('',(0.,0.,-1.));
#9874=DIRECTION('center_axis',(0.,0.,1.));
#9875=DIRECTION('ref_axis',(1.,0.,0.));
#9876=DIRECTION('center_axis',(0.,0.,1.));
#9877=DIRECTION('ref_axis',(1.,0.,0.));
#9878=DIRECTION('center_axis',(0.,0.,1.));
#9879=DIRECTION('ref_axis',(1.,0.,0.));
#9880=DIRECTION('center_axis',(0.,0.,1.));
#9881=DIRECTION('ref_axis',(1.,0.,0.));
#9882=DIRECTION('center_axis',(0.,0.,1.));
#9883=DIRECTION('ref_axis',(1.,0.,0.));
#9884=DIRECTION('',(0.,0.,-1.));
#9885=DIRECTION('center_axis',(0.,0.,1.));
#9886=DIRECTION('ref_axis',(1.,0.,0.));
#9887=DIRECTION('center_axis',(0.,0.,1.));
#9888=DIRECTION('ref_axis',(1.,0.,0.));
#9889=DIRECTION('center_axis',(0.,0.,1.));
#9890=DIRECTION('ref_axis',(1.,0.,0.));
#9891=DIRECTION('center_axis',(1.,0.,0.));
#9892=DIRECTION('ref_axis',(0.,0.,-1.));
#9893=DIRECTION('',(0.,1.,0.));
#9894=DIRECTION('center_axis',(1.,0.,0.));
#9895=DIRECTION('ref_axis',(0.,0.,-1.));
#9896=DIRECTION('center_axis',(1.,0.,0.));
#9897=DIRECTION('ref_axis',(0.,0.,-1.));
#9898=DIRECTION('center_axis',(1.,0.,0.));
#9899=DIRECTION('ref_axis',(0.,0.,-1.));
#9900=DIRECTION('',(1.,0.,0.));
#9901=DIRECTION('center_axis',(-1.,0.,0.));
#9902=DIRECTION('ref_axis',(0.,0.,-1.));
#9903=DIRECTION('center_axis',(1.,0.,0.));
#9904=DIRECTION('ref_axis',(0.,0.,-1.));
#9905=DIRECTION('center_axis',(1.,0.,0.));
#9906=DIRECTION('ref_axis',(0.,0.,-1.));
#9907=DIRECTION('',(0.,-1.,0.));
#9908=DIRECTION('center_axis',(0.,1.,0.));
#9909=DIRECTION('ref_axis',(1.,0.,0.));
#9910=DIRECTION('center_axis',(0.,1.,0.));
#9911=DIRECTION('ref_axis',(1.,0.,0.));
#9912=DIRECTION('',(0.,1.,0.));
#9913=DIRECTION('center_axis',(0.,-1.,0.));
#9914=DIRECTION('ref_axis',(1.,0.,0.));
#9915=DIRECTION('center_axis',(0.,-1.,0.));
#9916=DIRECTION('ref_axis',(1.,0.,0.));
#9917=DIRECTION('',(1.,0.,0.));
#9918=DIRECTION('',(0.,0.,1.));
#9919=DIRECTION('',(1.,0.,0.));
#9920=DIRECTION('',(0.,0.,1.));
#9921=DIRECTION('center_axis',(-1.,0.,0.));
#9922=DIRECTION('ref_axis',(0.,-1.,0.));
#9923=DIRECTION('',(0.,0.,-1.));
#9924=DIRECTION('',(0.,-1.,0.));
#9925=DIRECTION('',(0.,-1.,0.));
#9926=DIRECTION('center_axis',(0.,0.,1.));
#9927=DIRECTION('ref_axis',(1.,0.,0.));
#9928=DIRECTION('',(-1.,0.,0.));
#9929=DIRECTION('',(0.,1.,0.));
#9930=DIRECTION('center_axis',(0.,0.,1.));
#9931=DIRECTION('ref_axis',(1.,0.,0.));
#9932=DIRECTION('',(1.,0.,0.));
#9933=DIRECTION('',(0.,1.,0.));
#9934=DIRECTION('center_axis',(1.,0.,0.));
#9935=DIRECTION('ref_axis',(0.,1.,0.));
#9936=DIRECTION('',(0.,0.,1.));
#9937=DIRECTION('center_axis',(0.,1.,0.));
#9938=DIRECTION('ref_axis',(1.,0.,0.));
#9939=DIRECTION('axis',(0.,0.,1.));
#9940=DIRECTION('refdir',(1.,0.,0.));
#9941=DIRECTION('center_axis',(0.,1.,0.));
#9942=DIRECTION('ref_axis',(1.,0.,0.));
#9943=DIRECTION('center_axis',(0.,1.,0.));
#9944=DIRECTION('ref_axis',(1.,0.,0.));
#9945=DIRECTION('center_axis',(0.,1.,0.));
#9946=DIRECTION('ref_axis',(1.,0.,0.));
#9947=DIRECTION('center_axis',(0.,1.,0.));
#9948=DIRECTION('ref_axis',(1.,0.,0.));
#9949=DIRECTION('',(0.,-1.,0.));
#9950=DIRECTION('center_axis',(0.,1.,0.));
#9951=DIRECTION('ref_axis',(1.,0.,0.));
#9952=DIRECTION('center_axis',(0.,1.,0.));
#9953=DIRECTION('ref_axis',(1.,0.,0.));
#9954=DIRECTION('center_axis',(0.,1.,0.));
#9955=DIRECTION('ref_axis',(1.,0.,0.));
#9956=DIRECTION('center_axis',(0.,1.,0.));
#9957=DIRECTION('ref_axis',(1.,0.,0.));
#9958=DIRECTION('',(0.,-1.,0.));
#9959=DIRECTION('center_axis',(0.,1.,0.));
#9960=DIRECTION('ref_axis',(1.,0.,0.));
#9961=DIRECTION('axis',(0.,0.,1.));
#9962=DIRECTION('refdir',(1.,0.,0.));
#9963=DIRECTION('center_axis',(0.,0.,1.));
#9964=DIRECTION('ref_axis',(1.,0.,0.));
#9965=DIRECTION('center_axis',(0.,0.,1.));
#9966=DIRECTION('ref_axis',(1.,0.,0.));
#9967=DIRECTION('',(0.,0.,-1.));
#9968=DIRECTION('center_axis',(0.,0.,1.));
#9969=DIRECTION('ref_axis',(1.,0.,0.));
#9970=DIRECTION('center_axis',(0.,0.,1.));
#9971=DIRECTION('ref_axis',(1.,0.,0.));
#9972=DIRECTION('center_axis',(0.,0.,1.));
#9973=DIRECTION('ref_axis',(1.,0.,0.));
#9974=DIRECTION('axis',(0.,0.,1.));
#9975=DIRECTION('refdir',(1.,0.,0.));
#9976=DIRECTION('center_axis',(0.866025403784439,0.,-0.5));
#9977=DIRECTION('ref_axis',(0.5,0.,0.866025403784439));
#9978=DIRECTION('',(0.5,0.,0.866025403784439));
#9979=DIRECTION('',(0.,-1.,0.));
#9980=DIRECTION('',(0.5,0.,0.866025403784439));
#9981=DIRECTION('',(0.,-1.,0.));
#9982=DIRECTION('center_axis',(1.20185167898973E-16,0.,-1.));
#9983=DIRECTION('ref_axis',(1.,0.,1.20185167898973E-16));
#9984=DIRECTION('',(1.,0.,1.20185167898973E-16));
#9985=DIRECTION('',(0.,-1.,0.));
#9986=DIRECTION('',(1.,0.,1.20185167898973E-16));
#9987=DIRECTION('center_axis',(-0.866025403784439,0.,-0.5));
#9988=DIRECTION('ref_axis',(0.5,0.,-0.866025403784439));
#9989=DIRECTION('',(0.5,0.,-0.866025403784439));
#9990=DIRECTION('',(0.,-1.,0.));
#9991=DIRECTION('',(0.5,0.,-0.866025403784439));
#9992=DIRECTION('center_axis',(-0.866025403784439,0.,0.5));
#9993=DIRECTION('ref_axis',(-0.5,0.,-0.866025403784439));
#9994=DIRECTION('',(-0.5,0.,-0.866025403784439));
#9995=DIRECTION('',(0.,-1.,0.));
#9996=DIRECTION('',(-0.5,0.,-0.866025403784439));
#9997=DIRECTION('center_axis',(-2.40370335797945E-16,0.,1.));
#9998=DIRECTION('ref_axis',(-1.,0.,-2.40370335797945E-16));
#9999=DIRECTION('',(-1.,0.,-2.40370335797945E-16));
#10000=DIRECTION('',(0.,-1.,0.));
#10001=DIRECTION('',(-1.,0.,-2.40370335797945E-16));
#10002=DIRECTION('center_axis',(0.866025403784439,0.,0.5));
#10003=DIRECTION('ref_axis',(-0.5,0.,0.866025403784439));
#10004=DIRECTION('',(-0.5,0.,0.866025403784439));
#10005=DIRECTION('',(-0.5,0.,0.866025403784439));
#10006=DIRECTION('center_axis',(0.,-1.,0.));
#10007=DIRECTION('ref_axis',(0.,0.,-1.));
#10008=DIRECTION('center_axis',(0.,1.,0.));
#10009=DIRECTION('ref_axis',(0.,0.,1.));
#10010=DIRECTION('center_axis',(0.,-1.,0.));
#10011=DIRECTION('ref_axis',(1.,0.,0.));
#10012=DIRECTION('center_axis',(0.,-1.,0.));
#10013=DIRECTION('ref_axis',(1.,0.,0.));
#10014=DIRECTION('center_axis',(0.,-1.,0.));
#10015=DIRECTION('ref_axis',(1.,0.,0.));
#10016=DIRECTION('',(0.707106781186548,0.707106781186547,8.65956056235494E-17));
#10017=DIRECTION('center_axis',(0.,-1.,0.));
#10018=DIRECTION('ref_axis',(1.,0.,0.));
#10019=DIRECTION('center_axis',(0.,1.,0.));
#10020=DIRECTION('ref_axis',(1.,0.,0.));
#10021=DIRECTION('',(0.,1.,0.));
#10022=DIRECTION('center_axis',(0.,1.,0.));
#10023=DIRECTION('ref_axis',(1.,0.,0.));
#10024=DIRECTION('center_axis',(0.,-1.,0.));
#10025=DIRECTION('ref_axis',(1.,0.,0.));
#10026=DIRECTION('',(-0.707106781186548,0.707106781186547,-8.65956056235494E-17));
#10027=DIRECTION('center_axis',(0.,-1.,0.));
#10028=DIRECTION('ref_axis',(0.,0.,-1.));
#10029=DIRECTION('',(0.,0.,1.));
#10030=DIRECTION('',(1.,0.,0.));
#10031=DIRECTION('',(0.,0.,1.));
#10032=DIRECTION('',(1.,0.,0.));
#10033=DIRECTION('',(0.,0.,1.));
#10034=DIRECTION('',(1.,0.,0.));
#10035=DIRECTION('',(0.,0.,1.));
#10036=DIRECTION('',(2.22044604925031E-16,-1.,0.));
#10037=DIRECTION('',(0.,0.,1.));
#10038=DIRECTION('',(1.,0.,0.));
#10039=DIRECTION('',(0.,0.,1.));
#10040=DIRECTION('',(1.,0.,0.));
#10041=DIRECTION('',(0.,0.,1.));
#10042=DIRECTION('',(1.,0.,0.));
#10043=DIRECTION('',(0.,0.,1.));
#10044=DIRECTION('',(1.,0.,0.));
#10045=CARTESIAN_POINT('',(0.,0.,0.));
#10046=CARTESIAN_POINT('',(0.,0.,0.));
#10047=CARTESIAN_POINT('',(0.,0.,0.));
#10048=CARTESIAN_POINT('Origin',(1.5,-4.5,-0.1));
#10049=CARTESIAN_POINT('',(1.275,-4.5,0.));
#10050=CARTESIAN_POINT('Origin',(1.5,-4.5,0.));
#10051=CARTESIAN_POINT('',(1.275,-4.5,1.));
#10052=CARTESIAN_POINT('',(1.275,-4.5,-0.1));
#10053=CARTESIAN_POINT('Origin',(1.5,-4.5,1.));
#10054=CARTESIAN_POINT('Origin',(1.5,2.,-0.1));
#10055=CARTESIAN_POINT('',(1.275,2.,0.));
#10056=CARTESIAN_POINT('Origin',(1.5,2.,0.));
#10057=CARTESIAN_POINT('',(1.275,2.,1.));
#10058=CARTESIAN_POINT('',(1.275,2.,-0.1));
#10059=CARTESIAN_POINT('Origin',(1.5,2.,1.));
#10060=CARTESIAN_POINT('Origin',(-1.5,-4.5,-0.1));
#10061=CARTESIAN_POINT('',(-1.725,-4.5,0.));
#10062=CARTESIAN_POINT('Origin',(-1.5,-4.5,0.));
#10063=CARTESIAN_POINT('',(-1.725,-4.5,1.));
#10064=CARTESIAN_POINT('',(-1.725,-4.5,-0.1));
#10065=CARTESIAN_POINT('Origin',(-1.5,-4.5,1.));
#10066=CARTESIAN_POINT('Origin',(-1.5,2.,-0.1));
#10067=CARTESIAN_POINT('',(-1.725,2.,0.));
#10068=CARTESIAN_POINT('Origin',(-1.5,2.,0.));
#10069=CARTESIAN_POINT('',(-1.725,2.,1.));
#10070=CARTESIAN_POINT('',(-1.725,2.,-0.1));
#10071=CARTESIAN_POINT('Origin',(-1.5,2.,1.));
#10072=CARTESIAN_POINT('Origin',(-6.,-1.4,-0.1));
#10073=CARTESIAN_POINT('',(-6.21,-1.4,0.));
#10074=CARTESIAN_POINT('Origin',(-6.,-1.4,0.));
#10075=CARTESIAN_POINT('',(-6.21,-1.4,1.));
#10076=CARTESIAN_POINT('',(-6.21,-1.4,-0.1));
#10077=CARTESIAN_POINT('Origin',(-6.,-1.4,1.));
#10078=CARTESIAN_POINT('Origin',(-8.5,1.4,-0.1));
#10079=CARTESIAN_POINT('',(-8.71,1.4,0.));
#10080=CARTESIAN_POINT('Origin',(-8.5,1.4,0.));
#10081=CARTESIAN_POINT('',(-8.71,1.4,1.));
#10082=CARTESIAN_POINT('',(-8.71,1.4,-0.1));
#10083=CARTESIAN_POINT('Origin',(-8.5,1.4,1.));
#10084=CARTESIAN_POINT('Origin',(-8.5,-1.4,-0.1));
#10085=CARTESIAN_POINT('',(-8.71,-1.4,0.));
#10086=CARTESIAN_POINT('Origin',(-8.5,-1.4,0.));
#10087=CARTESIAN_POINT('',(-8.71,-1.4,1.));
#10088=CARTESIAN_POINT('',(-8.71,-1.4,-0.1));
#10089=CARTESIAN_POINT('Origin',(-8.5,-1.4,1.));
#10090=CARTESIAN_POINT('Origin',(-6.,1.4,-0.1));
#10091=CARTESIAN_POINT('',(-6.21,1.4,0.));
#10092=CARTESIAN_POINT('Origin',(-6.,1.4,0.));
#10093=CARTESIAN_POINT('',(-6.21,1.4,1.));
#10094=CARTESIAN_POINT('',(-6.21,1.4,-0.1));
#10095=CARTESIAN_POINT('Origin',(-6.,1.4,1.));
#10096=CARTESIAN_POINT('Origin',(3.5,4.5,0.));
#10097=CARTESIAN_POINT('',(3.5,4.5,0.));
#10098=CARTESIAN_POINT('',(-9.5,4.5,0.));
#10099=CARTESIAN_POINT('',(3.5,4.5,0.));
#10100=CARTESIAN_POINT('',(-9.5,4.5,1.));
#10101=CARTESIAN_POINT('',(-9.5,4.5,0.));
#10102=CARTESIAN_POINT('',(3.5,4.5,1.));
#10103=CARTESIAN_POINT('',(3.5,4.5,1.));
#10104=CARTESIAN_POINT('',(3.5,4.5,0.));
#10105=CARTESIAN_POINT('Origin',(3.5,-7.,0.));
#10106=CARTESIAN_POINT('',(3.5,-7.,0.));
#10107=CARTESIAN_POINT('',(3.5,-7.,0.));
#10108=CARTESIAN_POINT('',(3.5,-7.,1.));
#10109=CARTESIAN_POINT('',(3.5,-7.,1.));
#10110=CARTESIAN_POINT('',(3.5,-7.,0.));
#10111=CARTESIAN_POINT('Origin',(-9.5,-7.,0.));
#10112=CARTESIAN_POINT('',(-9.5,-7.,0.));
#10113=CARTESIAN_POINT('',(-9.5,-7.,0.));
#10114=CARTESIAN_POINT('',(-9.5,-7.,1.));
#10115=CARTESIAN_POINT('',(-9.5,-7.,1.));
#10116=CARTESIAN_POINT('',(-9.5,-7.,0.));
#10117=CARTESIAN_POINT('Origin',(-9.5,4.5,0.));
#10118=CARTESIAN_POINT('',(-9.5,4.5,0.));
#10119=CARTESIAN_POINT('',(-9.5,4.5,1.));
#10120=CARTESIAN_POINT('Origin',(-3.,-1.25,1.));
#10121=CARTESIAN_POINT('Origin',(-3.,-1.25,0.));
#10122=CARTESIAN_POINT('',(0.,0.,0.));
#10123=CARTESIAN_POINT('Origin',(3.5,-6.2,-0.8));
#10124=CARTESIAN_POINT('',(3.5,-6.2,-0.8));
#10125=CARTESIAN_POINT('',(-9.5,-6.2,-0.8));
#10126=CARTESIAN_POINT('',(3.5,-6.2,-0.8));
#10127=CARTESIAN_POINT('',(-9.5,-6.2,0.));
#10128=CARTESIAN_POINT('',(-9.5,-6.2,-0.8));
#10129=CARTESIAN_POINT('',(3.5,-6.2,0.));
#10130=CARTESIAN_POINT('',(3.5,-6.2,0.));
#10131=CARTESIAN_POINT('',(3.5,-6.2,-0.8));
#10132=CARTESIAN_POINT('Origin',(3.5,-7.,-0.8));
#10133=CARTESIAN_POINT('',(3.5,-7.,-0.8));
#10134=CARTESIAN_POINT('',(3.5,-7.,-0.8));
#10135=CARTESIAN_POINT('',(3.5,-7.,0.));
#10136=CARTESIAN_POINT('',(3.5,-7.,0.));
#10137=CARTESIAN_POINT('',(3.5,-7.,-0.8));
#10138=CARTESIAN_POINT('Origin',(-9.5,-7.,-0.8));
#10139=CARTESIAN_POINT('',(-9.5,-7.,-0.8));
#10140=CARTESIAN_POINT('',(-9.5,-7.,-0.8));
#10141=CARTESIAN_POINT('',(-9.5,-7.,0.));
#10142=CARTESIAN_POINT('',(-9.5,-7.,0.));
#10143=CARTESIAN_POINT('',(-9.5,-7.,-0.8));
#10144=CARTESIAN_POINT('Origin',(-9.5,-6.2,-0.8));
#10145=CARTESIAN_POINT('',(-9.5,-6.2,-0.8));
#10146=CARTESIAN_POINT('',(-9.5,-6.2,0.));
#10147=CARTESIAN_POINT('Origin',(-3.,-6.6,0.));
#10148=CARTESIAN_POINT('Origin',(-3.,-6.6,-0.8));
#10149=CARTESIAN_POINT('',(0.,0.,0.));
#10150=CARTESIAN_POINT('Origin',(3.5,4.5,-0.8));
#10151=CARTESIAN_POINT('',(3.5,4.5,-0.8));
#10152=CARTESIAN_POINT('',(-9.5,4.5,-0.8));
#10153=CARTESIAN_POINT('',(3.5,4.5,-0.8));
#10154=CARTESIAN_POINT('',(-9.5,4.5,0.));
#10155=CARTESIAN_POINT('',(-9.5,4.5,-0.8));
#10156=CARTESIAN_POINT('',(3.5,4.5,0.));
#10157=CARTESIAN_POINT('',(3.5,4.5,0.));
#10158=CARTESIAN_POINT('',(3.5,4.5,-0.8));
#10159=CARTESIAN_POINT('Origin',(3.5,3.7,-0.8));
#10160=CARTESIAN_POINT('',(3.5,3.7,-0.8));
#10161=CARTESIAN_POINT('',(3.5,3.7,-0.8));
#10162=CARTESIAN_POINT('',(3.5,3.7,0.));
#10163=CARTESIAN_POINT('',(3.5,3.7,0.));
#10164=CARTESIAN_POINT('',(3.5,3.7,-0.8));
#10165=CARTESIAN_POINT('Origin',(-9.5,3.7,-0.8));
#10166=CARTESIAN_POINT('',(-9.5,3.7,-0.8));
#10167=CARTESIAN_POINT('',(-9.5,3.7,-0.8));
#10168=CARTESIAN_POINT('',(-9.5,3.7,0.));
#10169=CARTESIAN_POINT('',(-9.5,3.7,0.));
#10170=CARTESIAN_POINT('',(-9.5,3.7,-0.8));
#10171=CARTESIAN_POINT('Origin',(-9.5,4.5,-0.8));
#10172=CARTESIAN_POINT('',(-9.5,4.5,-0.8));
#10173=CARTESIAN_POINT('',(-9.5,4.5,0.));
#10174=CARTESIAN_POINT('Origin',(-3.,4.1,0.));
#10175=CARTESIAN_POINT('Origin',(-3.,4.1,-0.8));
#10176=CARTESIAN_POINT('',(0.,0.,0.));
#10177=CARTESIAN_POINT('Origin',(-5.25982293614231,-0.9,14.8604204653858));
#10178=CARTESIAN_POINT('',(-5.48482293614231,-0.8,14.8604204653858));
#10179=CARTESIAN_POINT('Origin',(-5.25982293614231,-0.8,14.8604204653858));
#10180=CARTESIAN_POINT('',(-5.48482293614231,0.8,14.8604204653858));
#10181=CARTESIAN_POINT('',(-5.48482293614231,-0.9,14.8604204653858));
#10182=CARTESIAN_POINT('Origin',(-5.25982293614231,0.8,14.8604204653858));
#10183=CARTESIAN_POINT('Origin',(-1.13137084989848,-1.13137084989848,15.8));
#10184=CARTESIAN_POINT('',(-1.29637084989848,-1.13137084989848,15.8));
#10185=CARTESIAN_POINT('Origin',(-1.13137084989848,-1.13137084989848,15.8));
#10186=CARTESIAN_POINT('',(-1.29637084989848,-1.13137084989848,16.5));
#10187=CARTESIAN_POINT('',(-1.29637084989848,-1.13137084989848,15.8));
#10188=CARTESIAN_POINT('Origin',(-1.13137084989848,-1.13137084989848,16.5));
#10189=CARTESIAN_POINT('Origin',(-1.13137084989848,-1.13137084989848,15.8));
#10190=CARTESIAN_POINT('Origin',(-1.13137084989848,1.13137084989848,15.8));
#10191=CARTESIAN_POINT('',(-1.29637084989848,1.13137084989848,15.8));
#10192=CARTESIAN_POINT('Origin',(-1.13137084989848,1.13137084989848,15.8));
#10193=CARTESIAN_POINT('',(-1.29637084989848,1.13137084989848,16.5));
#10194=CARTESIAN_POINT('',(-1.29637084989848,1.13137084989848,15.8));
#10195=CARTESIAN_POINT('Origin',(-1.13137084989848,1.13137084989848,16.5));
#10196=CARTESIAN_POINT('Origin',(-1.13137084989848,1.13137084989848,15.8));
#10197=CARTESIAN_POINT('Origin',(1.13137084989848,1.13137084989848,15.8));
#10198=CARTESIAN_POINT('',(0.966370849898476,1.13137084989848,15.8));
#10199=CARTESIAN_POINT('Origin',(1.13137084989848,1.13137084989848,15.8));
#10200=CARTESIAN_POINT('',(0.966370849898476,1.13137084989848,16.5));
#10201=CARTESIAN_POINT('',(0.966370849898476,1.13137084989848,15.8));
#10202=CARTESIAN_POINT('Origin',(1.13137084989848,1.13137084989848,16.5));
#10203=CARTESIAN_POINT('Origin',(1.13137084989848,1.13137084989848,15.8));
#10204=CARTESIAN_POINT('Origin',(1.13137084989848,-1.13137084989848,15.8));
#10205=CARTESIAN_POINT('',(0.966370849898476,-1.13137084989848,15.8));
#10206=CARTESIAN_POINT('Origin',(1.13137084989848,-1.13137084989848,15.8));
#10207=CARTESIAN_POINT('',(0.966370849898476,-1.13137084989848,16.5));
#10208=CARTESIAN_POINT('',(0.966370849898476,-1.13137084989848,15.8));
#10209=CARTESIAN_POINT('Origin',(1.13137084989848,-1.13137084989848,16.5));
#10210=CARTESIAN_POINT('Origin',(1.13137084989848,-1.13137084989848,15.8));
#10211=CARTESIAN_POINT('Origin',(-5.23743686707646,-0.9,9.76256313292354));
#10212=CARTESIAN_POINT('',(-5.40243686707646,-0.8,9.76256313292354));
#10213=CARTESIAN_POINT('Origin',(-5.23743686707646,-0.8,9.76256313292354));
#10214=CARTESIAN_POINT('',(-5.40243686707646,0.8,9.76256313292354));
#10215=CARTESIAN_POINT('',(-5.40243686707646,-0.9,9.76256313292354));
#10216=CARTESIAN_POINT('Origin',(-5.23743686707646,0.8,9.76256313292354));
#10217=CARTESIAN_POINT('Origin',(-5.23743686707646,-0.9,12.2374368670765));
#10218=CARTESIAN_POINT('',(-5.40243686707646,-0.8,12.2374368670765));
#10219=CARTESIAN_POINT('Origin',(-5.23743686707646,-0.8,12.2374368670765));
#10220=CARTESIAN_POINT('',(-5.40243686707646,0.8,12.2374368670765));
#10221=CARTESIAN_POINT('',(-5.40243686707646,-0.9,12.2374368670765));
#10222=CARTESIAN_POINT('Origin',(-5.23743686707646,0.8,12.2374368670765));
#10223=CARTESIAN_POINT('Origin',(-2.76256313292354,-0.9,12.2374368670765));
#10224=CARTESIAN_POINT('',(-2.92756313292354,-0.8,12.2374368670765));
#10225=CARTESIAN_POINT('Origin',(-2.76256313292354,-0.8,12.2374368670765));
#10226=CARTESIAN_POINT('',(-2.92756313292354,0.8,12.2374368670765));
#10227=CARTESIAN_POINT('',(-2.92756313292354,-0.9,12.2374368670765));
#10228=CARTESIAN_POINT('Origin',(-2.76256313292354,0.8,12.2374368670765));
#10229=CARTESIAN_POINT('Origin',(-2.76256313292354,-0.9,9.76256313292354));
#10230=CARTESIAN_POINT('',(-2.92756313292354,-0.8,9.76256313292354));
#10231=CARTESIAN_POINT('Origin',(-2.76256313292354,-0.8,9.76256313292354));
#10232=CARTESIAN_POINT('',(-2.92756313292354,0.8,9.76256313292354));
#10233=CARTESIAN_POINT('',(-2.92756313292354,-0.9,9.76256313292354));
#10234=CARTESIAN_POINT('Origin',(-2.76256313292354,0.8,9.76256313292354));
#10235=CARTESIAN_POINT('Origin',(-6.,-1.4,0.9));
#10236=CARTESIAN_POINT('',(-6.275,-1.4,1.));
#10237=CARTESIAN_POINT('Origin',(-6.,-1.4,1.));
#10238=CARTESIAN_POINT('',(-6.275,-1.4,1.8));
#10239=CARTESIAN_POINT('',(-6.275,-1.4,0.9));
#10240=CARTESIAN_POINT('Origin',(-6.,-1.4,1.8));
#10241=CARTESIAN_POINT('Origin',(-8.5,1.4,0.9));
#10242=CARTESIAN_POINT('',(-8.775,1.4,1.));
#10243=CARTESIAN_POINT('Origin',(-8.5,1.4,1.));
#10244=CARTESIAN_POINT('',(-8.775,1.4,1.8));
#10245=CARTESIAN_POINT('',(-8.775,1.4,0.9));
#10246=CARTESIAN_POINT('Origin',(-8.5,1.4,1.8));
#10247=CARTESIAN_POINT('Origin',(-8.5,-1.4,0.9));
#10248=CARTESIAN_POINT('',(-8.775,-1.4,1.));
#10249=CARTESIAN_POINT('Origin',(-8.5,-1.4,1.));
#10250=CARTESIAN_POINT('',(-8.775,-1.4,1.8));
#10251=CARTESIAN_POINT('',(-8.775,-1.4,0.9));
#10252=CARTESIAN_POINT('Origin',(-8.5,-1.4,1.8));
#10253=CARTESIAN_POINT('Origin',(-6.,1.4,0.9));
#10254=CARTESIAN_POINT('',(-6.275,1.4,1.));
#10255=CARTESIAN_POINT('Origin',(-6.,1.4,1.));
#10256=CARTESIAN_POINT('',(-6.275,1.4,1.8));
#10257=CARTESIAN_POINT('',(-6.275,1.4,0.9));
#10258=CARTESIAN_POINT('Origin',(-6.,1.4,1.8));
#10259=CARTESIAN_POINT('Origin',(0.,0.,12.5));
#10260=CARTESIAN_POINT('',(-1.05,-1.28587913910472E-16,12.5));
#10261=CARTESIAN_POINT('Origin',(0.,0.,12.5));
#10262=CARTESIAN_POINT('',(-1.05,1.28587913910472E-16,16.5));
#10263=CARTESIAN_POINT('',(-1.05,-1.28587913910472E-16,12.5));
#10264=CARTESIAN_POINT('Origin',(0.,0.,16.5));
#10265=CARTESIAN_POINT('Origin',(0.,0.,12.5));
#10266=CARTESIAN_POINT('',(-0.625,-7.65404249467096E-17,12.5));
#10267=CARTESIAN_POINT('Origin',(0.,0.,12.5));
#10268=CARTESIAN_POINT('Origin',(0.,0.,11.9));
#10269=CARTESIAN_POINT('',(-0.625,-7.65404249467096E-17,12.));
#10270=CARTESIAN_POINT('Origin',(0.,0.,12.));
#10271=CARTESIAN_POINT('',(-0.625,-7.65404249467096E-17,11.9));
#10272=CARTESIAN_POINT('Origin',(-4.,-0.9,11.));
#10273=CARTESIAN_POINT('',(-5.5,-0.8,11.));
#10274=CARTESIAN_POINT('Origin',(-4.,-0.8,11.));
#10275=CARTESIAN_POINT('',(-5.5,0.8,11.));
#10276=CARTESIAN_POINT('',(-5.5,-0.9,11.));
#10277=CARTESIAN_POINT('Origin',(-4.,0.8,11.));
#10278=CARTESIAN_POINT('Origin',(0.,0.,12.));
#10279=CARTESIAN_POINT('',(-1.83303027798234,-0.8,12.));
#10280=CARTESIAN_POINT('',(-1.83303027798234,-0.8,16.5));
#10281=CARTESIAN_POINT('',(-1.83303027798234,-0.8,12.));
#10282=CARTESIAN_POINT('',(-1.83303027798234,0.8,12.));
#10283=CARTESIAN_POINT('Origin',(0.,0.,12.));
#10284=CARTESIAN_POINT('',(-1.83303027798234,0.8,16.5));
#10285=CARTESIAN_POINT('',(-1.83303027798234,0.8,12.));
#10286=CARTESIAN_POINT('Origin',(0.,0.,16.5));
#10287=CARTESIAN_POINT('Origin',(-8.,-0.8,1.));
#10288=CARTESIAN_POINT('',(-6.5,-0.8,16.5));
#10289=CARTESIAN_POINT('',(1.5,-0.8,16.5));
#10290=CARTESIAN_POINT('',(-6.5,-0.8,17.5));
#10291=CARTESIAN_POINT('',(-6.5,-0.8,1.));
#10292=CARTESIAN_POINT('',(-8.,-0.8,17.5));
#10293=CARTESIAN_POINT('',(-8.,-0.8,17.5));
#10294=CARTESIAN_POINT('',(-8.,-0.8,1.8));
#10295=CARTESIAN_POINT('',(-8.,-0.8,1.));
#10296=CARTESIAN_POINT('',(-6.5,-0.8,1.8));
#10297=CARTESIAN_POINT('',(-7.625,-0.8,1.8));
#10298=CARTESIAN_POINT('',(-6.5,-0.8,12.));
#10299=CARTESIAN_POINT('',(-6.5,-0.8,1.));
#10300=CARTESIAN_POINT('',(-5.95959179422654,-0.8,12.));
#10301=CARTESIAN_POINT('',(-8.,-0.8,12.));
#10302=CARTESIAN_POINT('',(-2.04040820577346,-0.8,12.));
#10303=CARTESIAN_POINT('Origin',(-4.,-0.8,11.));
#10304=CARTESIAN_POINT('',(-8.,-0.8,12.));
#10305=CARTESIAN_POINT('Origin',(-8.,-0.8,16.5));
#10306=CARTESIAN_POINT('',(-6.5,0.8,16.5));
#10307=CARTESIAN_POINT('',(1.5,0.8,16.5));
#10308=CARTESIAN_POINT('',(-6.5,-0.8,16.5));
#10309=CARTESIAN_POINT('Origin',(-7.25,0.,1.8));
#10310=CARTESIAN_POINT('',(-9.,2.,1.8));
#10311=CARTESIAN_POINT('',(-9.,-2.,1.8));
#10312=CARTESIAN_POINT('',(-9.,2.,1.8));
#10313=CARTESIAN_POINT('',(-5.5,-2.,1.8));
#10314=CARTESIAN_POINT('',(-9.,-2.,1.8));
#10315=CARTESIAN_POINT('',(-5.5,2.,1.8));
#10316=CARTESIAN_POINT('',(-5.5,-2.,1.8));
#10317=CARTESIAN_POINT('',(-5.5,2.,1.8));
#10318=CARTESIAN_POINT('',(-6.5,0.8,1.8));
#10319=CARTESIAN_POINT('',(-8.,0.8,1.8));
#10320=CARTESIAN_POINT('',(-6.875,0.8,1.8));
#10321=CARTESIAN_POINT('',(-6.5,-0.4,1.8));
#10322=CARTESIAN_POINT('',(-8.,0.4,1.8));
#10323=CARTESIAN_POINT('Origin',(-5.5,2.,1.));
#10324=CARTESIAN_POINT('',(-5.5,2.,1.));
#10325=CARTESIAN_POINT('',(-9.,2.,1.));
#10326=CARTESIAN_POINT('',(-5.5,2.,1.));
#10327=CARTESIAN_POINT('',(-9.,2.,1.));
#10328=CARTESIAN_POINT('',(-5.5,2.,1.));
#10329=CARTESIAN_POINT('Origin',(-5.5,-2.,1.));
#10330=CARTESIAN_POINT('',(-5.5,-2.,1.));
#10331=CARTESIAN_POINT('',(-5.5,-2.,1.));
#10332=CARTESIAN_POINT('',(-5.5,-2.,1.));
#10333=CARTESIAN_POINT('Origin',(-9.,-2.,1.));
#10334=CARTESIAN_POINT('',(-9.,-2.,1.));
#10335=CARTESIAN_POINT('',(-9.,-2.,1.));
#10336=CARTESIAN_POINT('',(-9.,-2.,1.));
#10337=CARTESIAN_POINT('Origin',(-9.,2.,1.));
#10338=CARTESIAN_POINT('',(-9.,2.,1.));
#10339=CARTESIAN_POINT('Origin',(-6.5,-0.8,1.));
#10340=CARTESIAN_POINT('',(-6.5,0.8,12.));
#10341=CARTESIAN_POINT('',(-6.5,0.8,1.));
#10342=CARTESIAN_POINT('',(-6.5,-0.8,12.));
#10343=CARTESIAN_POINT('Origin',(-4.,-0.8,11.));
#10344=CARTESIAN_POINT('',(-2.04040820577346,0.8,12.));
#10345=CARTESIAN_POINT('',(-2.04040820577346,-0.8,12.));
#10346=CARTESIAN_POINT('',(-5.95959179422654,0.8,12.));
#10347=CARTESIAN_POINT('',(-5.95959179422654,-0.8,12.));
#10348=CARTESIAN_POINT('Origin',(-4.,0.8,11.));
#10349=CARTESIAN_POINT('Origin',(-6.5,0.8,1.));
#10350=CARTESIAN_POINT('',(-8.,0.8,12.));
#10351=CARTESIAN_POINT('',(-8.,0.8,12.));
#10352=CARTESIAN_POINT('',(-8.,0.8,17.5));
#10353=CARTESIAN_POINT('',(-8.,0.8,1.));
#10354=CARTESIAN_POINT('',(-6.5,0.8,17.5));
#10355=CARTESIAN_POINT('',(-6.5,0.8,17.5));
#10356=CARTESIAN_POINT('',(-6.5,0.8,1.));
#10357=CARTESIAN_POINT('Origin',(1.5,-0.8,12.));
#10358=CARTESIAN_POINT('Origin',(1.5,-0.8,12.));
#10359=CARTESIAN_POINT('Origin',(-6.5,-0.8,1.));
#10360=CARTESIAN_POINT('',(-6.5,-0.8,17.5));
#10361=CARTESIAN_POINT('Origin',(-8.,0.8,1.));
#10362=CARTESIAN_POINT('',(-8.,0.8,17.5));
#10363=CARTESIAN_POINT('Origin',(-7.25,0.,17.5));
#10364=CARTESIAN_POINT('Origin',(-7.25,0.,1.));
#10365=CARTESIAN_POINT('',(0.,0.,0.));
#10366=CARTESIAN_POINT('Origin',(-5.23743686707646,-1.1,9.76256313292354));
#10367=CARTESIAN_POINT('',(-5.46243686707646,-1.,9.76256313292354));
#10368=CARTESIAN_POINT('Origin',(-5.23743686707646,-1.,9.76256313292354));
#10369=CARTESIAN_POINT('',(-5.46243686707646,-0.8,9.76256313292354));
#10370=CARTESIAN_POINT('',(-5.46243686707646,-1.1,9.76256313292354));
#10371=CARTESIAN_POINT('Origin',(-5.23743686707646,-0.8,9.76256313292354));
#10372=CARTESIAN_POINT('Origin',(-5.23743686707646,-1.1,12.2374368670765));
#10373=CARTESIAN_POINT('',(-5.46243686707646,-1.,12.2374368670765));
#10374=CARTESIAN_POINT('Origin',(-5.23743686707646,-1.,12.2374368670765));
#10375=CARTESIAN_POINT('',(-5.46243686707646,-0.8,12.2374368670765));
#10376=CARTESIAN_POINT('',(-5.46243686707646,-1.1,12.2374368670765));
#10377=CARTESIAN_POINT('Origin',(-5.23743686707646,-0.8,12.2374368670765));
#10378=CARTESIAN_POINT('Origin',(-2.76256313292354,-1.1,12.2374368670765));
#10379=CARTESIAN_POINT('',(-2.98756313292354,-1.,12.2374368670765));
#10380=CARTESIAN_POINT('Origin',(-2.76256313292354,-1.,12.2374368670765));
#10381=CARTESIAN_POINT('',(-2.98756313292354,-0.8,12.2374368670765));
#10382=CARTESIAN_POINT('',(-2.98756313292354,-1.1,12.2374368670765));
#10383=CARTESIAN_POINT('Origin',(-2.76256313292354,-0.8,12.2374368670765));
#10384=CARTESIAN_POINT('Origin',(-2.76256313292354,-1.1,9.76256313292354));
#10385=CARTESIAN_POINT('',(-2.98756313292354,-1.,9.76256313292354));
#10386=CARTESIAN_POINT('Origin',(-2.76256313292354,-1.,9.76256313292354));
#10387=CARTESIAN_POINT('',(-2.98756313292354,-0.8,9.76256313292354));
#10388=CARTESIAN_POINT('',(-2.98756313292354,-1.1,9.76256313292354));
#10389=CARTESIAN_POINT('Origin',(-2.76256313292354,-0.8,9.76256313292354));
#10390=CARTESIAN_POINT('Origin',(-4.,-0.8,11.));
#10391=CARTESIAN_POINT('',(-5.49,-0.45,11.));
#10392=CARTESIAN_POINT('Origin',(-4.,-0.45,11.));
#10393=CARTESIAN_POINT('',(-5.49,-0.8,11.));
#10394=CARTESIAN_POINT('',(-5.49,-0.8,11.));
#10395=CARTESIAN_POINT('Origin',(-4.,-0.8,11.));
#10396=CARTESIAN_POINT('Origin',(-4.,-0.45,11.));
#10397=CARTESIAN_POINT('',(-4.71,-0.45,11.));
#10398=CARTESIAN_POINT('Origin',(-4.,-0.45,11.));
#10399=CARTESIAN_POINT('Origin',(-4.,-1.,11.));
#10400=CARTESIAN_POINT('',(-4.71,-1.,11.));
#10401=CARTESIAN_POINT('',(-4.71,-1.,11.));
#10402=CARTESIAN_POINT('Origin',(-4.,-1.,11.));
#10403=CARTESIAN_POINT('Origin',(-4.,-1.,11.));
#10404=CARTESIAN_POINT('',(-6.2,-0.8,11.));
#10405=CARTESIAN_POINT('Origin',(-4.,-0.8,11.));
#10406=CARTESIAN_POINT('',(-6.2,-1.,11.));
#10407=CARTESIAN_POINT('',(-6.2,-1.,11.));
#10408=CARTESIAN_POINT('Origin',(-4.,-1.,11.));
#10409=CARTESIAN_POINT('Origin',(-4.,-0.8,11.));
#10410=CARTESIAN_POINT('Origin',(-4.,-1.,11.));
#10411=CARTESIAN_POINT('',(0.,0.,0.));
#10412=CARTESIAN_POINT('Origin',(-5.23743686707646,0.7,9.76256313292354));
#10413=CARTESIAN_POINT('',(-5.46243686707646,0.8,9.76256313292354));
#10414=CARTESIAN_POINT('Origin',(-5.23743686707646,0.8,9.76256313292354));
#10415=CARTESIAN_POINT('',(-5.46243686707646,1.,9.76256313292354));
#10416=CARTESIAN_POINT('',(-5.46243686707646,0.7,9.76256313292354));
#10417=CARTESIAN_POINT('Origin',(-5.23743686707646,1.,9.76256313292354));
#10418=CARTESIAN_POINT('Origin',(-5.23743686707646,0.7,12.2374368670765));
#10419=CARTESIAN_POINT('',(-5.46243686707646,0.8,12.2374368670765));
#10420=CARTESIAN_POINT('Origin',(-5.23743686707646,0.8,12.2374368670765));
#10421=CARTESIAN_POINT('',(-5.46243686707646,1.,12.2374368670765));
#10422=CARTESIAN_POINT('',(-5.46243686707646,0.7,12.2374368670765));
#10423=CARTESIAN_POINT('Origin',(-5.23743686707646,1.,12.2374368670765));
#10424=CARTESIAN_POINT('Origin',(-2.76256313292354,0.7,12.2374368670765));
#10425=CARTESIAN_POINT('',(-2.98756313292354,0.8,12.2374368670765));
#10426=CARTESIAN_POINT('Origin',(-2.76256313292354,0.8,12.2374368670765));
#10427=CARTESIAN_POINT('',(-2.98756313292354,1.,12.2374368670765));
#10428=CARTESIAN_POINT('',(-2.98756313292354,0.7,12.2374368670765));
#10429=CARTESIAN_POINT('Origin',(-2.76256313292354,1.,12.2374368670765));
#10430=CARTESIAN_POINT('Origin',(-2.76256313292354,0.7,9.76256313292354));
#10431=CARTESIAN_POINT('',(-2.98756313292354,0.8,9.76256313292354));
#10432=CARTESIAN_POINT('Origin',(-2.76256313292354,0.8,9.76256313292354));
#10433=CARTESIAN_POINT('',(-2.98756313292354,1.,9.76256313292354));
#10434=CARTESIAN_POINT('',(-2.98756313292354,0.7,9.76256313292354));
#10435=CARTESIAN_POINT('Origin',(-2.76256313292354,1.,9.76256313292354));
#10436=CARTESIAN_POINT('Origin',(-4.,0.45,11.));
#10437=CARTESIAN_POINT('',(-5.49,0.8,11.));
#10438=CARTESIAN_POINT('Origin',(-4.,0.8,11.));
#10439=CARTESIAN_POINT('',(-5.49,0.45,11.));
#10440=CARTESIAN_POINT('',(-5.49,0.45,11.));
#10441=CARTESIAN_POINT('Origin',(-4.,0.45,11.));
#10442=CARTESIAN_POINT('Origin',(-4.,0.45,11.));
#10443=CARTESIAN_POINT('',(-4.71,0.45,11.));
#10444=CARTESIAN_POINT('Origin',(-4.,0.45,11.));
#10445=CARTESIAN_POINT('Origin',(-4.,0.8,11.));
#10446=CARTESIAN_POINT('',(-4.71,1.,11.));
#10447=CARTESIAN_POINT('Origin',(-4.,1.,11.));
#10448=CARTESIAN_POINT('',(-4.71,0.8,11.));
#10449=CARTESIAN_POINT('Origin',(-4.,0.8,11.));
#10450=CARTESIAN_POINT('',(-6.2,1.,11.));
#10451=CARTESIAN_POINT('Origin',(-4.,1.,11.));
#10452=CARTESIAN_POINT('',(-6.2,0.8,11.));
#10453=CARTESIAN_POINT('',(-6.2,0.8,11.));
#10454=CARTESIAN_POINT('Origin',(-4.,0.8,11.));
#10455=CARTESIAN_POINT('Origin',(-4.,1.,11.));
#10456=CARTESIAN_POINT('Origin',(-4.,0.8,11.));
#10457=CARTESIAN_POINT('',(0.,0.,0.));
#10458=CARTESIAN_POINT('Origin',(-1.13137084989848,-1.13137084989848,16.9));
#10459=CARTESIAN_POINT('',(-1.50637084989848,-1.13137084989848,16.9));
#10460=CARTESIAN_POINT('Origin',(-1.13137084989848,-1.13137084989848,16.9));
#10461=CARTESIAN_POINT('',(-1.50637084989848,-1.13137084989848,17.3));
#10462=CARTESIAN_POINT('',(-1.50637084989848,-1.13137084989848,16.9));
#10463=CARTESIAN_POINT('Origin',(-1.13137084989848,-1.13137084989848,17.3));
#10464=CARTESIAN_POINT('Origin',(-1.13137084989848,-1.13137084989848,16.9));
#10465=CARTESIAN_POINT('',(-1.35637084989848,-1.13137084989848,16.9));
#10466=CARTESIAN_POINT('Origin',(-1.13137084989848,-1.13137084989848,16.9));
#10467=CARTESIAN_POINT('Origin',(-1.13137084989848,1.13137084989848,16.9));
#10468=CARTESIAN_POINT('',(-1.50637084989848,1.13137084989848,16.9));
#10469=CARTESIAN_POINT('Origin',(-1.13137084989848,1.13137084989848,16.9));
#10470=CARTESIAN_POINT('',(-1.50637084989848,1.13137084989848,17.3));
#10471=CARTESIAN_POINT('',(-1.50637084989848,1.13137084989848,16.9));
#10472=CARTESIAN_POINT('Origin',(-1.13137084989848,1.13137084989848,17.3));
#10473=CARTESIAN_POINT('Origin',(-1.13137084989848,1.13137084989848,16.9));
#10474=CARTESIAN_POINT('',(-1.35637084989848,1.13137084989848,16.9));
#10475=CARTESIAN_POINT('Origin',(-1.13137084989848,1.13137084989848,16.9));
#10476=CARTESIAN_POINT('Origin',(1.13137084989848,1.13137084989848,16.9));
#10477=CARTESIAN_POINT('',(0.756370849898476,1.13137084989848,16.9));
#10478=CARTESIAN_POINT('Origin',(1.13137084989848,1.13137084989848,16.9));
#10479=CARTESIAN_POINT('',(0.756370849898476,1.13137084989848,17.3));
#10480=CARTESIAN_POINT('',(0.756370849898476,1.13137084989848,16.9));
#10481=CARTESIAN_POINT('Origin',(1.13137084989848,1.13137084989848,17.3));
#10482=CARTESIAN_POINT('Origin',(1.13137084989848,1.13137084989848,16.9));
#10483=CARTESIAN_POINT('',(0.906370849898476,1.13137084989848,16.9));
#10484=CARTESIAN_POINT('Origin',(1.13137084989848,1.13137084989848,16.9));
#10485=CARTESIAN_POINT('Origin',(1.13137084989848,-1.13137084989848,16.9));
#10486=CARTESIAN_POINT('',(0.756370849898476,-1.13137084989848,16.9));
#10487=CARTESIAN_POINT('Origin',(1.13137084989848,-1.13137084989848,16.9));
#10488=CARTESIAN_POINT('',(0.756370849898476,-1.13137084989848,17.3));
#10489=CARTESIAN_POINT('',(0.756370849898476,-1.13137084989848,16.9));
#10490=CARTESIAN_POINT('Origin',(1.13137084989848,-1.13137084989848,17.3));
#10491=CARTESIAN_POINT('Origin',(1.13137084989848,-1.13137084989848,16.9));
#10492=CARTESIAN_POINT('',(0.906370849898476,-1.13137084989848,16.9));
#10493=CARTESIAN_POINT('Origin',(1.13137084989848,-1.13137084989848,16.9));
#10494=CARTESIAN_POINT('Origin',(-1.13137084989848,-1.13137084989848,16.4));
#10495=CARTESIAN_POINT('',(-1.35637084989848,-1.13137084989848,16.5));
#10496=CARTESIAN_POINT('Origin',(-1.13137084989848,-1.13137084989848,16.5));
#10497=CARTESIAN_POINT('',(-1.35637084989848,-1.13137084989848,16.4));
#10498=CARTESIAN_POINT('Origin',(-1.13137084989848,1.13137084989848,16.4));
#10499=CARTESIAN_POINT('',(-1.35637084989848,1.13137084989848,16.5));
#10500=CARTESIAN_POINT('Origin',(-1.13137084989848,1.13137084989848,16.5));
#10501=CARTESIAN_POINT('',(-1.35637084989848,1.13137084989848,16.4));
#10502=CARTESIAN_POINT('Origin',(1.13137084989848,1.13137084989848,16.4));
#10503=CARTESIAN_POINT('',(0.906370849898476,1.13137084989848,16.5));
#10504=CARTESIAN_POINT('Origin',(1.13137084989848,1.13137084989848,16.5));
#10505=CARTESIAN_POINT('',(0.906370849898476,1.13137084989848,16.4));
#10506=CARTESIAN_POINT('Origin',(1.13137084989848,-1.13137084989848,16.4));
#10507=CARTESIAN_POINT('',(0.906370849898476,-1.13137084989848,16.5));
#10508=CARTESIAN_POINT('Origin',(1.13137084989848,-1.13137084989848,16.5));
#10509=CARTESIAN_POINT('',(0.906370849898476,-1.13137084989848,16.4));
#10510=CARTESIAN_POINT('Origin',(0.,0.,15.5));
#10511=CARTESIAN_POINT('',(-1.04,-1.27363267111325E-16,16.5));
#10512=CARTESIAN_POINT('Origin',(0.,0.,16.5));
#10513=CARTESIAN_POINT('',(-1.04,-1.27363267111325E-16,15.5));
#10514=CARTESIAN_POINT('',(-1.04,-1.27363267111325E-16,15.5));
#10515=CARTESIAN_POINT('Origin',(0.,0.,15.5));
#10516=CARTESIAN_POINT('Origin',(0.,0.,15.5));
#10517=CARTESIAN_POINT('',(-0.625,-7.65404249467096E-17,15.5));
#10518=CARTESIAN_POINT('Origin',(0.,0.,15.5));
#10519=CARTESIAN_POINT('Origin',(0.,0.,16.5));
#10520=CARTESIAN_POINT('',(-0.625,-7.65404249467096E-17,17.3));
#10521=CARTESIAN_POINT('Origin',(0.,0.,17.3));
#10522=CARTESIAN_POINT('',(-0.625,-7.65404249467096E-17,16.5));
#10523=CARTESIAN_POINT('Origin',(0.,0.,16.5));
#10524=CARTESIAN_POINT('',(-2.,-2.44929359829471E-16,17.3));
#10525=CARTESIAN_POINT('Origin',(0.,0.,17.3));
#10526=CARTESIAN_POINT('',(-2.,-2.44929359829471E-16,16.5));
#10527=CARTESIAN_POINT('',(-2.,-2.44929359829471E-16,16.5));
#10528=CARTESIAN_POINT('Origin',(0.,0.,16.5));
#10529=CARTESIAN_POINT('Origin',(0.,0.,17.3));
#10530=CARTESIAN_POINT('Origin',(0.,0.,16.5));
#10531=CARTESIAN_POINT('',(0.,0.,0.));
#10532=CARTESIAN_POINT('Origin',(1.,3.5,1.));
#10533=CARTESIAN_POINT('',(1.,3.5,1.));
#10534=CARTESIAN_POINT('',(-1.,3.5,1.));
#10535=CARTESIAN_POINT('',(1.,3.5,1.));
#10536=CARTESIAN_POINT('',(-1.,3.5,3.));
#10537=CARTESIAN_POINT('',(-1.,3.5,1.));
#10538=CARTESIAN_POINT('',(1.,3.5,3.));
#10539=CARTESIAN_POINT('',(1.,3.5,3.));
#10540=CARTESIAN_POINT('',(1.,3.5,1.));
#10541=CARTESIAN_POINT('Origin',(1.,-6.,1.));
#10542=CARTESIAN_POINT('',(1.,-6.,1.));
#10543=CARTESIAN_POINT('',(1.,-6.,1.));
#10544=CARTESIAN_POINT('',(1.,-6.,3.));
#10545=CARTESIAN_POINT('',(1.,-6.,3.));
#10546=CARTESIAN_POINT('',(1.,-6.,1.));
#10547=CARTESIAN_POINT('Origin',(-1.,-6.,1.));
#10548=CARTESIAN_POINT('',(-1.,-6.,1.));
#10549=CARTESIAN_POINT('',(-1.,-6.,1.));
#10550=CARTESIAN_POINT('',(-1.,-6.,3.));
#10551=CARTESIAN_POINT('',(-1.,-6.,3.));
#10552=CARTESIAN_POINT('',(-1.,-6.,1.));
#10553=CARTESIAN_POINT('Origin',(-1.,3.5,1.));
#10554=CARTESIAN_POINT('',(-1.,3.5,1.));
#10555=CARTESIAN_POINT('',(-1.,3.5,3.));
#10556=CARTESIAN_POINT('Origin',(0.,-1.25,3.));
#10557=CARTESIAN_POINT('Origin',(0.,-1.25,1.));
#10558=CARTESIAN_POINT('',(0.,0.,0.));
#10559=CARTESIAN_POINT('Origin',(-1.5,-4.5,0.9));
#10560=CARTESIAN_POINT('',(-1.665,-4.5,1.));
#10561=CARTESIAN_POINT('Origin',(-1.5,-4.5,1.));
#10562=CARTESIAN_POINT('',(-1.665,-4.5,1.7));
#10563=CARTESIAN_POINT('',(-1.665,-4.5,0.9));
#10564=CARTESIAN_POINT('Origin',(-1.5,-4.5,1.7));
#10565=CARTESIAN_POINT('Origin',(-1.5,-4.5,1.7));
#10566=CARTESIAN_POINT('Origin',(-1.5,2.,0.9));
#10567=CARTESIAN_POINT('',(-1.665,2.,1.));
#10568=CARTESIAN_POINT('Origin',(-1.5,2.,1.));
#10569=CARTESIAN_POINT('',(-1.665,2.,1.7));
#10570=CARTESIAN_POINT('',(-1.665,2.,0.9));
#10571=CARTESIAN_POINT('Origin',(-1.5,2.,1.7));
#10572=CARTESIAN_POINT('Origin',(-1.5,2.,1.7));
#10573=CARTESIAN_POINT('Origin',(-1.01,3.5,1.));
#10574=CARTESIAN_POINT('',(-1.01,3.5,1.));
#10575=CARTESIAN_POINT('',(-2.,3.5,1.));
#10576=CARTESIAN_POINT('',(-1.01,3.5,1.));
#10577=CARTESIAN_POINT('',(-2.,3.5,2.5));
#10578=CARTESIAN_POINT('',(-2.,3.5,1.));
#10579=CARTESIAN_POINT('',(-1.01,3.5,2.5));
#10580=CARTESIAN_POINT('',(-1.01,3.5,2.5));
#10581=CARTESIAN_POINT('',(-1.01,3.5,1.));
#10582=CARTESIAN_POINT('Origin',(-1.01,-6.,1.));
#10583=CARTESIAN_POINT('',(-1.01,-6.,1.));
#10584=CARTESIAN_POINT('',(-1.01,-6.,1.));
#10585=CARTESIAN_POINT('',(-1.01,-6.,2.5));
#10586=CARTESIAN_POINT('',(-1.01,-6.,2.5));
#10587=CARTESIAN_POINT('',(-1.01,-6.,1.));
#10588=CARTESIAN_POINT('Origin',(-2.,-6.,1.));
#10589=CARTESIAN_POINT('',(-2.,-6.,1.));
#10590=CARTESIAN_POINT('',(-2.,-6.,1.));
#10591=CARTESIAN_POINT('',(-2.,-6.,2.5));
#10592=CARTESIAN_POINT('',(-2.,-6.,2.5));
#10593=CARTESIAN_POINT('',(-2.,-6.,1.));
#10594=CARTESIAN_POINT('Origin',(-2.,3.5,1.));
#10595=CARTESIAN_POINT('',(-2.,3.5,1.));
#10596=CARTESIAN_POINT('',(-2.,3.5,2.5));
#10597=CARTESIAN_POINT('Origin',(-1.505,-1.25,2.5));
#10598=CARTESIAN_POINT('Origin',(-1.505,-1.25,1.));
#10599=CARTESIAN_POINT('',(0.,0.,0.));
#10600=CARTESIAN_POINT('Origin',(1.5,-4.5,0.9));
#10601=CARTESIAN_POINT('',(1.335,-4.5,1.));
#10602=CARTESIAN_POINT('Origin',(1.5,-4.5,1.));
#10603=CARTESIAN_POINT('',(1.335,-4.5,1.7));
#10604=CARTESIAN_POINT('',(1.335,-4.5,0.9));
#10605=CARTESIAN_POINT('Origin',(1.5,-4.5,1.7));
#10606=CARTESIAN_POINT('Origin',(1.5,-4.5,1.7));
#10607=CARTESIAN_POINT('Origin',(1.5,2.,0.9));
#10608=CARTESIAN_POINT('',(1.335,2.,1.));
#10609=CARTESIAN_POINT('Origin',(1.5,2.,1.));
#10610=CARTESIAN_POINT('',(1.335,2.,1.7));
#10611=CARTESIAN_POINT('',(1.335,2.,0.9));
#10612=CARTESIAN_POINT('Origin',(1.5,2.,1.7));
#10613=CARTESIAN_POINT('Origin',(1.5,2.,1.7));
#10614=CARTESIAN_POINT('Origin',(2.,3.5,1.));
#10615=CARTESIAN_POINT('',(2.,3.5,1.));
#10616=CARTESIAN_POINT('',(1.01,3.5,1.));
#10617=CARTESIAN_POINT('',(2.,3.5,1.));
#10618=CARTESIAN_POINT('',(1.01,3.5,2.5));
#10619=CARTESIAN_POINT('',(1.01,3.5,1.));
#10620=CARTESIAN_POINT('',(2.,3.5,2.5));
#10621=CARTESIAN_POINT('',(2.,3.5,2.5));
#10622=CARTESIAN_POINT('',(2.,3.5,1.));
#10623=CARTESIAN_POINT('Origin',(2.,-6.,1.));
#10624=CARTESIAN_POINT('',(2.,-6.,1.));
#10625=CARTESIAN_POINT('',(2.,-6.,1.));
#10626=CARTESIAN_POINT('',(2.,-6.,2.5));
#10627=CARTESIAN_POINT('',(2.,-6.,2.5));
#10628=CARTESIAN_POINT('',(2.,-6.,1.));
#10629=CARTESIAN_POINT('Origin',(1.01,-6.,1.));
#10630=CARTESIAN_POINT('',(1.01,-6.,1.));
#10631=CARTESIAN_POINT('',(1.01,-6.,1.));
#10632=CARTESIAN_POINT('',(1.01,-6.,2.5));
#10633=CARTESIAN_POINT('',(1.01,-6.,2.5));
#10634=CARTESIAN_POINT('',(1.01,-6.,1.));
#10635=CARTESIAN_POINT('Origin',(1.01,3.5,1.));
#10636=CARTESIAN_POINT('',(1.01,3.5,1.));
#10637=CARTESIAN_POINT('',(1.01,3.5,2.5));
#10638=CARTESIAN_POINT('Origin',(1.505,-1.25,2.5));
#10639=CARTESIAN_POINT('Origin',(1.505,-1.25,1.));
#10640=CARTESIAN_POINT('',(0.,0.,0.));
#10641=CARTESIAN_POINT('Origin',(-5.25982293614231,-2.4,14.8604204653858));
#10642=CARTESIAN_POINT('',(-5.42482293614231,-2.4,14.8604204653858));
#10643=CARTESIAN_POINT('Origin',(-5.25982293614231,-2.4,14.8604204653858));
#10644=CARTESIAN_POINT('',(-5.42482293614231,-0.8,14.8604204653858));
#10645=CARTESIAN_POINT('',(-5.42482293614231,-2.4,14.8604204653858));
#10646=CARTESIAN_POINT('Origin',(-5.25982293614231,-0.8,14.8604204653858));
#10647=CARTESIAN_POINT('Origin',(-5.25982293614231,-2.4,14.8604204653858));
#10648=CARTESIAN_POINT('Origin',(-5.25982293614231,-2.3,14.8604204653858));
#10649=CARTESIAN_POINT('',(-5.75982293614231,-2.3,14.8604204653858));
#10650=CARTESIAN_POINT('Origin',(-5.25982293614231,-2.3,14.8604204653858));
#10651=CARTESIAN_POINT('',(-5.55982293614231,-2.3,14.8604204653858));
#10652=CARTESIAN_POINT('Origin',(-5.25982293614231,-2.3,14.8604204653858));
#10653=CARTESIAN_POINT('Origin',(-5.25982293614231,-2.3,14.8604204653858));
#10654=CARTESIAN_POINT('',(-5.75982293614231,-0.8,14.8604204653858));
#10655=CARTESIAN_POINT('Origin',(-5.25982293614231,-0.8,14.8604204653858));
#10656=CARTESIAN_POINT('',(-5.75982293614231,-2.3,14.8604204653858));
#10657=CARTESIAN_POINT('Origin',(-5.25982293614231,-0.8,14.8604204653858));
#10658=CARTESIAN_POINT('Origin',(-5.25982293614231,-3.9,14.8604204653858));
#10659=CARTESIAN_POINT('',(-5.55982293614231,-3.9,14.8604204653858));
#10660=CARTESIAN_POINT('',(-5.55982293614231,-3.9,14.8604204653858));
#10661=CARTESIAN_POINT('Origin',(-5.25982293614231,-3.9,14.8604204653858));
#10662=CARTESIAN_POINT('Origin',(-5.25982293614231,-3.9,14.8604204653858));
#10663=CARTESIAN_POINT('',(0.,0.,0.));
#10664=CARTESIAN_POINT('Origin',(0.115470053837925,-0.5,-0.2));
#10665=CARTESIAN_POINT('',(0.23094010767585,-0.5,0.));
#10666=CARTESIAN_POINT('',(0.115470053837925,-0.5,-0.2));
#10667=CARTESIAN_POINT('',(0.23094010767585,-0.5,0.));
#10668=CARTESIAN_POINT('',(0.115470053837925,-0.8,-0.2));
#10669=CARTESIAN_POINT('',(0.115470053837925,-0.5,-0.2));
#10670=CARTESIAN_POINT('',(0.23094010767585,-0.8,0.));
#10671=CARTESIAN_POINT('',(0.23094010767585,-0.8,0.));
#10672=CARTESIAN_POINT('',(0.23094010767585,-0.5,0.));
#10673=CARTESIAN_POINT('Origin',(-0.115470053837925,-0.5,-0.2));
#10674=CARTESIAN_POINT('',(-0.115470053837925,-0.5,-0.2));
#10675=CARTESIAN_POINT('',(0.115470053837925,-0.5,-0.2));
#10676=CARTESIAN_POINT('',(-0.115470053837925,-0.8,-0.2));
#10677=CARTESIAN_POINT('',(-0.115470053837925,-0.5,-0.2));
#10678=CARTESIAN_POINT('',(0.115470053837925,-0.8,-0.2));
#10679=CARTESIAN_POINT('Origin',(-0.23094010767585,-0.5,-2.77555756156289E-17));
#10680=CARTESIAN_POINT('',(-0.23094010767585,-0.5,-2.82820063659975E-17));
#10681=CARTESIAN_POINT('',(-0.115470053837925,-0.5,-0.2));
#10682=CARTESIAN_POINT('',(-0.23094010767585,-0.8,-2.77555756156289E-17));
#10683=CARTESIAN_POINT('',(-0.23094010767585,-0.5,-2.82820063659975E-17));
#10684=CARTESIAN_POINT('',(-0.115470053837925,-0.8,-0.2));
#10685=CARTESIAN_POINT('Origin',(-0.115470053837925,-0.5,0.2));
#10686=CARTESIAN_POINT('',(-0.115470053837925,-0.5,0.2));
#10687=CARTESIAN_POINT('',(-0.23094010767585,-0.5,-2.82820063659975E-17));
#10688=CARTESIAN_POINT('',(-0.115470053837925,-0.8,0.2));
#10689=CARTESIAN_POINT('',(-0.115470053837925,-0.5,0.2));
#10690=CARTESIAN_POINT('',(-0.23094010767585,-0.8,-2.82820063659975E-17));
#10691=CARTESIAN_POINT('Origin',(0.115470053837925,-0.5,0.2));
#10692=CARTESIAN_POINT('',(0.115470053837925,-0.5,0.2));
#10693=CARTESIAN_POINT('',(-0.115470053837925,-0.5,0.2));
#10694=CARTESIAN_POINT('',(0.115470053837925,-0.8,0.2));
#10695=CARTESIAN_POINT('',(0.115470053837925,-0.5,0.2));
#10696=CARTESIAN_POINT('',(-0.115470053837925,-0.8,0.2));
#10697=CARTESIAN_POINT('Origin',(0.23094010767585,-0.5,0.));
#10698=CARTESIAN_POINT('',(0.115470053837925,-0.5,0.2));
#10699=CARTESIAN_POINT('',(0.115470053837925,-0.8,0.2));
#10700=CARTESIAN_POINT('Origin',(0.,-0.5,0.));
#10701=CARTESIAN_POINT('Origin',(0.,-0.8,0.));
#10702=CARTESIAN_POINT('Origin',(0.,-1.4,0.));
#10703=CARTESIAN_POINT('',(-0.24505,-1.4,3.00099698131059E-17));
#10704=CARTESIAN_POINT('Origin',(0.,-1.4,0.));
#10705=CARTESIAN_POINT('Origin',(0.375,0.5,0.));
#10706=CARTESIAN_POINT('',(-0.375,0.5,-4.59242549680257E-17));
#10707=CARTESIAN_POINT('Origin',(0.,0.5,0.));
#10708=CARTESIAN_POINT('Origin',(0.,0.475,0.));
#10709=CARTESIAN_POINT('',(-0.425,0.45,-5.20474889637625E-17));
#10710=CARTESIAN_POINT('Origin',(0.,0.45,0.));
#10711=CARTESIAN_POINT('',(-0.4,0.475,-4.89858719658941E-17));
#10712=CARTESIAN_POINT('Origin',(0.,0.24,0.));
#10713=CARTESIAN_POINT('',(-0.425,0.0299999999999998,-5.20474889637625E-17));
#10714=CARTESIAN_POINT('Origin',(0.,0.0299999999999998,0.));
#10715=CARTESIAN_POINT('',(-0.425,0.24,-5.20474889637625E-17));
#10716=CARTESIAN_POINT('Origin',(0.,0.0150000000000001,0.));
#10717=CARTESIAN_POINT('',(-0.395,4.85722573273506E-17,-4.83735485663204E-17));
#10718=CARTESIAN_POINT('Origin',(0.,0.,0.));
#10719=CARTESIAN_POINT('',(-0.41,0.0150000000000001,-5.02105187650415E-17));
#10720=CARTESIAN_POINT('Origin',(0.27,0.,0.));
#10721=CARTESIAN_POINT('',(-0.27,0.,-3.30654635769785E-17));
#10722=CARTESIAN_POINT('Origin',(0.,0.,0.));
#10723=CARTESIAN_POINT('Origin',(0.,-0.02,0.));
#10724=CARTESIAN_POINT('',(-0.24505,-0.0498999999999999,3.00099698131059E-17));
#10725=CARTESIAN_POINT('Origin',(0.,-0.0498999999999999,0.));
#10726=CARTESIAN_POINT('',(-0.26,-0.02,-3.18408167778312E-17));
#10727=CARTESIAN_POINT('Origin',(0.,-0.995,0.));
#10728=CARTESIAN_POINT('',(-0.24505,-0.995,-3.00099698131059E-17));
#10729=CARTESIAN_POINT('',(0.,0.,0.));
#10730=CARTESIAN_POINT('',(0.,0.,0.));
#10731=CARTESIAN_POINT('Origin',(0.,0.,0.));
#10732=CARTESIAN_POINT('',(-0.976185,-0.246528389340863,-1.19548183562566E-16));
#10733=CARTESIAN_POINT('',(-1.19548183562566E-16,-0.246528389340863,0.976185));
#10734=CARTESIAN_POINT('Origin',(0.,-0.246528389340863,0.));
#10735=CARTESIAN_POINT('Origin',(0.,-0.246528389340863,0.));
#10736=CARTESIAN_POINT('',(-1.19548183562566E-16,0.246528389340863,0.976185));
#10737=CARTESIAN_POINT('Origin',(-1.22464679914735E-16,0.,1.));
#10738=CARTESIAN_POINT('',(-0.976185,0.246528389340863,1.19548183562566E-16));
#10739=CARTESIAN_POINT('Origin',(0.,0.246528389340863,0.));
#10740=CARTESIAN_POINT('Origin',(0.,0.246528389340863,0.));
#10741=CARTESIAN_POINT('Origin',(0.,0.,0.));
#10742=CARTESIAN_POINT('',(-0.976185,0.45,-1.19548183562566E-16));
#10743=CARTESIAN_POINT('',(-0.976185,0.,-1.19548183562566E-16));
#10744=CARTESIAN_POINT('Origin',(0.,0.45,0.));
#10745=CARTESIAN_POINT('Origin',(0.,0.,0.));
#10746=CARTESIAN_POINT('',(-0.5,-0.39,-6.12323399573677E-17));
#10747=CARTESIAN_POINT('Origin',(0.,-0.39,0.));
#10748=CARTESIAN_POINT('',(-0.5,0.39,-6.12323399573677E-17));
#10749=CARTESIAN_POINT('',(-0.5,0.,-6.12323399573677E-17));
#10750=CARTESIAN_POINT('Origin',(0.,0.39,0.));
#10751=CARTESIAN_POINT('Origin',(0.,0.42,0.));
#10752=CARTESIAN_POINT('',(-0.56,0.45,-6.85802207522518E-17));
#10753=CARTESIAN_POINT('',(-0.53,0.42,-6.49062803548097E-17));
#10754=CARTESIAN_POINT('Origin',(0.,0.45,0.));
#10755=CARTESIAN_POINT('Origin',(0.976185,0.45,0.));
#10756=CARTESIAN_POINT('Origin',(0.,0.,0.));
#10757=CARTESIAN_POINT('',(-0.976185,-0.45,-1.19548183562566E-16));
#10758=CARTESIAN_POINT('Origin',(0.,-0.45,0.));
#10759=CARTESIAN_POINT('',(-0.976185,0.,-1.19548183562566E-16));
#10760=CARTESIAN_POINT('Origin',(0.56,-0.45,0.));
#10761=CARTESIAN_POINT('',(-0.56,-0.45,-6.85802207522518E-17));
#10762=CARTESIAN_POINT('Origin',(0.,-0.45,0.));
#10763=CARTESIAN_POINT('Origin',(0.,-0.42,0.));
#10764=CARTESIAN_POINT('',(-0.53,-0.42,-6.49062803548097E-17));
#10765=CARTESIAN_POINT('',(0.,0.,0.));
#10766=CARTESIAN_POINT('Origin',(0.,0.,0.));
#10767=CARTESIAN_POINT('',(-1.023815,0.246528389340863,-1.25381176266905E-16));
#10768=CARTESIAN_POINT('',(-1.25381176266905E-16,0.246528389340863,1.023815));
#10769=CARTESIAN_POINT('Origin',(0.,0.246528389340863,0.));
#10770=CARTESIAN_POINT('Origin',(0.,0.246528389340863,0.));
#10771=CARTESIAN_POINT('',(-1.25381176266905E-16,-0.246528389340863,1.023815));
#10772=CARTESIAN_POINT('Origin',(-1.22464679914735E-16,0.,1.));
#10773=CARTESIAN_POINT('',(-1.023815,-0.246528389340863,1.25381176266905E-16));
#10774=CARTESIAN_POINT('Origin',(0.,-0.246528389340863,0.));
#10775=CARTESIAN_POINT('Origin',(0.,-0.246528389340863,0.));
#10776=CARTESIAN_POINT('Origin',(0.,0.,0.));
#10777=CARTESIAN_POINT('',(-1.023815,-0.45,-1.25381176266905E-16));
#10778=CARTESIAN_POINT('Origin',(0.,-0.45,0.));
#10779=CARTESIAN_POINT('',(-1.023815,0.,-1.25381176266905E-16));
#10780=CARTESIAN_POINT('Origin',(1.44,0.45,0.));
#10781=CARTESIAN_POINT('',(-1.44,0.45,-1.76349139077219E-16));
#10782=CARTESIAN_POINT('Origin',(0.,0.45,0.));
#10783=CARTESIAN_POINT('',(-1.023815,0.45,-1.25381176266905E-16));
#10784=CARTESIAN_POINT('Origin',(0.,0.45,0.));
#10785=CARTESIAN_POINT('Origin',(0.,0.42,0.));
#10786=CARTESIAN_POINT('',(-1.5,0.39,-1.83697019872103E-16));
#10787=CARTESIAN_POINT('Origin',(0.,0.39,0.));
#10788=CARTESIAN_POINT('',(-1.47,0.42,-1.80023079474661E-16));
#10789=CARTESIAN_POINT('Origin',(0.,0.,0.));
#10790=CARTESIAN_POINT('',(-1.5,-0.39,-1.83697019872103E-16));
#10791=CARTESIAN_POINT('Origin',(0.,-0.39,0.));
#10792=CARTESIAN_POINT('',(-1.5,0.,-1.83697019872103E-16));
#10793=CARTESIAN_POINT('Origin',(0.,-0.42,0.));
#10794=CARTESIAN_POINT('',(-1.44,-0.45,-1.76349139077219E-16));
#10795=CARTESIAN_POINT('Origin',(0.,-0.45,0.));
#10796=CARTESIAN_POINT('',(-1.47,-0.42,-1.80023079474661E-16));
#10797=CARTESIAN_POINT('Origin',(1.023815,-0.45,0.));
#10798=CARTESIAN_POINT('Origin',(0.,0.,0.));
#10799=CARTESIAN_POINT('',(-1.023815,0.,-1.25381176266905E-16));
#10800=CARTESIAN_POINT('',(0.,0.,0.));
#10801=CARTESIAN_POINT('Origin',(1.,0.,0.));
#10802=CARTESIAN_POINT('',(1.,-1.78583896120461E-33,0.23815));
#10803=CARTESIAN_POINT('',(1.,-1.78583896120461E-33,-0.23815));
#10804=CARTESIAN_POINT('Origin',(1.,0.,0.));
#10805=CARTESIAN_POINT('Origin',(0.707106781186548,0.,-0.707106781186547));
#10806=CARTESIAN_POINT('',(0.875504261126124,-1.78583896120461E-33,-0.538709301246971));
#10807=CARTESIAN_POINT('',(0.538709301246971,-1.78583896120461E-33,-0.875504261126124));
#10808=CARTESIAN_POINT('Origin',(0.707106781186548,0.,-0.707106781186547));
#10809=CARTESIAN_POINT('Origin',(6.12323399573677E-17,0.,-1.));
#10810=CARTESIAN_POINT('',(0.23815,-1.78583896120461E-33,-1.));
#10811=CARTESIAN_POINT('',(-0.23815,-1.78583896120461E-33,-1.));
#10812=CARTESIAN_POINT('Origin',(6.12323399573677E-17,0.,-1.));
#10813=CARTESIAN_POINT('Origin',(-0.707106781186547,0.,-0.707106781186548));
#10814=CARTESIAN_POINT('',(-0.538709301246971,-1.78583896120461E-33,-0.875504261126124));
#10815=CARTESIAN_POINT('',(-0.875504261126124,-1.78583896120461E-33,-0.538709301246971));
#10816=CARTESIAN_POINT('Origin',(-0.707106781186547,0.,-0.707106781186548));
#10817=CARTESIAN_POINT('Origin',(-1.,0.,-1.22464679914735E-16));
#10818=CARTESIAN_POINT('',(-1.,-1.78583896120461E-33,-0.23815));
#10819=CARTESIAN_POINT('',(-1.,-1.78583896120461E-33,0.23815));
#10820=CARTESIAN_POINT('Origin',(-1.,0.,-1.22464679914735E-16));
#10821=CARTESIAN_POINT('Origin',(-0.707106781186548,0.,0.707106781186547));
#10822=CARTESIAN_POINT('',(-0.875504261126124,-7.94881478324376E-33,0.538709301246971));
#10823=CARTESIAN_POINT('',(-0.538709301246971,4.37713686083455E-33,0.875504261126124));
#10824=CARTESIAN_POINT('Origin',(-0.707106781186548,0.,0.707106781186547));
#10825=CARTESIAN_POINT('Origin',(-1.83697019872103E-16,0.,1.));
#10826=CARTESIAN_POINT('',(-0.23815,-1.78583896120461E-33,1.));
#10827=CARTESIAN_POINT('',(0.23815,-1.78583896120461E-33,1.));
#10828=CARTESIAN_POINT('Origin',(-1.83697019872103E-16,0.,1.));
#10829=CARTESIAN_POINT('Origin',(0.707106781186547,0.,0.707106781186548));
#10830=CARTESIAN_POINT('',(0.538709301246971,-4.86732687222419E-33,0.875504261126124));
#10831=CARTESIAN_POINT('',(0.875504261126124,1.29564894981497E-33,0.538709301246971));
#10832=CARTESIAN_POINT('Origin',(0.707106781186547,0.,0.707106781186548));
#10833=CARTESIAN_POINT('',(0.,0.,0.));
#10834=CARTESIAN_POINT('Origin',(0.707106781186547,0.,0.707106781186548));
#10835=CARTESIAN_POINT('',(0.504455939115715,-0.04763,0.841298510752802));
#10836=CARTESIAN_POINT('',(0.841298510752802,-0.04763,0.504455939115715));
#10837=CARTESIAN_POINT('Ctrl Pts',(0.504455939115715,-0.04763,0.841298510752802));
#10838=CARTESIAN_POINT('Ctrl Pts',(0.508899795931835,-0.0740444353928835,
0.838633903678357));
#10839=CARTESIAN_POINT('Ctrl Pts',(0.517157748491652,-0.0999305678883309,
0.833661031856294));
#10840=CARTESIAN_POINT('Ctrl Pts',(0.537715343527944,-0.142345102874864,
0.820511285096538));
#10841=CARTESIAN_POINT('Ctrl Pts',(0.548874290046456,-0.159766064500479,
0.813159949759));
#10842=CARTESIAN_POINT('Ctrl Pts',(0.573915184558107,-0.190326085855194,
0.795684265985089));
#10843=CARTESIAN_POINT('Ctrl Pts',(0.587792702767295,-0.203463743702801,
0.78555112003688));
#10844=CARTESIAN_POINT('Ctrl Pts',(0.615966552324775,-0.224161999508995,
0.763642258217233));
#10845=CARTESIAN_POINT('Ctrl Pts',(0.631684198665438,-0.232861760990032,
0.750785745543687));
#10846=CARTESIAN_POINT('Ctrl Pts',(0.663382628119203,-0.244251601209411,
0.722929908501543));
#10847=CARTESIAN_POINT('Ctrl Pts',(0.679352081686668,-0.246942143572133,
0.707917883896095));
#10848=CARTESIAN_POINT('Ctrl Pts',(0.707917883896095,-0.246942143572133,
0.679352081686668));
#10849=CARTESIAN_POINT('Ctrl Pts',(0.722929908501543,-0.244251601209411,
0.663382628119203));
#10850=CARTESIAN_POINT('Ctrl Pts',(0.750785745543687,-0.232861760990032,
0.631684198665439));
#10851=CARTESIAN_POINT('Ctrl Pts',(0.763642258217232,-0.224161999508995,
0.615966552324775));
#10852=CARTESIAN_POINT('Ctrl Pts',(0.78555112003688,-0.203463743702801,
0.587792702767295));
#10853=CARTESIAN_POINT('Ctrl Pts',(0.795684265985088,-0.190326085855194,
0.573915184558108));
#10854=CARTESIAN_POINT('Ctrl Pts',(0.813159949759,-0.15976606450048,0.548874290046456));
#10855=CARTESIAN_POINT('Ctrl Pts',(0.820511285096538,-0.142345102874864,
0.537715343527944));
#10856=CARTESIAN_POINT('Ctrl Pts',(0.833661031856294,-0.099930567888331,
0.517157748491653));
#10857=CARTESIAN_POINT('Ctrl Pts',(0.838633903678357,-0.0740444353928835,
0.508899795931835));
#10858=CARTESIAN_POINT('Ctrl Pts',(0.841298510752801,-0.0476299999999999,
0.504455939115715));
#10859=CARTESIAN_POINT('',(0.528110872004958,-0.04763,0.871530771444223));
#10860=CARTESIAN_POINT('Origin',(0.707106781186547,-0.04763,0.707106781186548));
#10861=CARTESIAN_POINT('',(0.871530771444223,-0.04763,0.528110872004959));
#10862=CARTESIAN_POINT('Ctrl Pts',(0.871530771444223,-0.0476300000000001,
0.528110872004958));
#10863=CARTESIAN_POINT('Ctrl Pts',(0.87014664509073,-0.0609922781173483,
0.530395067942936));
#10864=CARTESIAN_POINT('Ctrl Pts',(0.868149331745851,-0.0742967091364493,
0.533674141594226));
#10865=CARTESIAN_POINT('Ctrl Pts',(0.85981294420286,-0.115492077056649,
0.54708917182331));
#10866=CARTESIAN_POINT('Ctrl Pts',(0.850993704737257,-0.141695629206859,
0.560922177770136));
#10867=CARTESIAN_POINT('Ctrl Pts',(0.830754510485543,-0.181890537957859,
0.590422647829571));
#10868=CARTESIAN_POINT('Ctrl Pts',(0.816896541396381,-0.201072148666545,
0.609616703125488));
#10869=CARTESIAN_POINT('Ctrl Pts',(0.792310597819928,-0.223955109275652,
0.641117951819998));
#10870=CARTESIAN_POINT('Ctrl Pts',(0.779109323683612,-0.232742381310829,
0.657208095763053));
#10871=CARTESIAN_POINT('Ctrl Pts',(0.750552691816206,-0.244234834628584,
0.68964083160521));
#10872=CARTESIAN_POINT('Ctrl Pts',(0.735185187071673,-0.246942143572133,
0.705971972091755));
#10873=CARTESIAN_POINT('Ctrl Pts',(0.705971972091754,-0.246942143572133,
0.735185187071673));
#10874=CARTESIAN_POINT('Ctrl Pts',(0.689640831605209,-0.244234834628584,
0.750552691816206));
#10875=CARTESIAN_POINT('Ctrl Pts',(0.657208095763052,-0.232742381310829,
0.779109323683612));
#10876=CARTESIAN_POINT('Ctrl Pts',(0.641117951819998,-0.223955109275652,
0.792310597819928));
#10877=CARTESIAN_POINT('Ctrl Pts',(0.609616703125487,-0.201072148666545,
0.816896541396382));
#10878=CARTESIAN_POINT('Ctrl Pts',(0.590422647829571,-0.181890537957858,
0.830754510485544));
#10879=CARTESIAN_POINT('Ctrl Pts',(0.560922177770135,-0.141695629206858,
0.850993704737257));
#10880=CARTESIAN_POINT('Ctrl Pts',(0.547089171823309,-0.115492077056649,
0.859812944202861));
#10881=CARTESIAN_POINT('Ctrl Pts',(0.533674141594226,-0.0742967091364491,
0.868149331745852));
#10882=CARTESIAN_POINT('Ctrl Pts',(0.530395067942936,-0.0609922781173483,
0.870146645090731));
#10883=CARTESIAN_POINT('Ctrl Pts',(0.528110872004958,-0.0476300000000001,
0.871530771444223));
#10884=CARTESIAN_POINT('Origin',(0.707106781186547,-0.04763,0.707106781186548));
#10885=CARTESIAN_POINT('Origin',(0.,-0.166705,0.));
#10886=CARTESIAN_POINT('',(0.242834539687906,-0.04763,0.989696097314));
#10887=CARTESIAN_POINT('Origin',(0.,-0.04763,0.));
#10888=CARTESIAN_POINT('',(-0.242834539687907,-0.04763,0.989696097314));
#10889=CARTESIAN_POINT('Ctrl Pts',(0.242834539687906,-0.04763,0.989696097314));
#10890=CARTESIAN_POINT('Ctrl Pts',(0.24024064412003,-0.0609922781173483,
0.990332542620729));
#10891=CARTESIAN_POINT('Ctrl Pts',(0.236509675094874,-0.0742967091364492,
0.991238884025248));
#10892=CARTESIAN_POINT('Ctrl Pts',(0.221129100087819,-0.115492077056649,
0.994830026707808));
#10893=CARTESIAN_POINT('Ctrl Pts',(0.205111543747588,-0.141695629206859,
0.998375294985966));
#10894=CARTESIAN_POINT('Ctrl Pts',(0.169940289819232,-0.181890537957859,
1.00492400591205));
#10895=CARTESIAN_POINT('Ctrl Pts',(0.1465689792446,-0.201072148666545,1.00869718865384));
#10896=CARTESIAN_POINT('Ctrl Pts',(0.106909345252087,-0.223955109275652,
1.01358704779679));
#10897=CARTESIAN_POINT('Ctrl Pts',(0.0861971848975941,-0.232742381310829,
1.0156297872271));
#10898=CARTESIAN_POINT('Ctrl Pts',(0.0430711894098822,-0.244234834628584,
1.01837060663223));
#10899=CARTESIAN_POINT('Ctrl Pts',(0.0206568624125605,-0.246942143572133,
1.019052));
#10900=CARTESIAN_POINT('Ctrl Pts',(-0.0206568624125608,-0.246942143572133,
1.019052));
#10901=CARTESIAN_POINT('Ctrl Pts',(-0.0430711894098825,-0.244234834628584,
1.01837060663223));
#10902=CARTESIAN_POINT('Ctrl Pts',(-0.0861971848975943,-0.232742381310829,
1.0156297872271));
#10903=CARTESIAN_POINT('Ctrl Pts',(-0.106909345252088,-0.223955109275652,
1.01358704779679));
#10904=CARTESIAN_POINT('Ctrl Pts',(-0.1465689792446,-0.201072148666545,
1.00869718865384));
#10905=CARTESIAN_POINT('Ctrl Pts',(-0.169940289819232,-0.181890537957859,
1.00492400591205));
#10906=CARTESIAN_POINT('Ctrl Pts',(-0.205111543747588,-0.141695629206859,
0.998375294985966));
#10907=CARTESIAN_POINT('Ctrl Pts',(-0.221129100087819,-0.115492077056649,
0.994830026707808));
#10908=CARTESIAN_POINT('Ctrl Pts',(-0.236509675094875,-0.0742967091364493,
0.991238884025248));
#10909=CARTESIAN_POINT('Ctrl Pts',(-0.24024064412003,-0.0609922781173483,
0.990332542620729));
#10910=CARTESIAN_POINT('Ctrl Pts',(-0.242834539687907,-0.04763,0.989696097314));
#10911=CARTESIAN_POINT('',(-0.528110872004959,-0.04763,0.871530771444223));
#10912=CARTESIAN_POINT('Origin',(0.,-0.04763,0.));
#10913=CARTESIAN_POINT('',(-0.871530771444223,-0.04763,0.528110872004958));
#10914=CARTESIAN_POINT('Ctrl Pts',(-0.528110872004958,-0.0476300000000001,
0.871530771444223));
#10915=CARTESIAN_POINT('Ctrl Pts',(-0.530395067942936,-0.0609922781173484,
0.87014664509073));
#10916=CARTESIAN_POINT('Ctrl Pts',(-0.533674141594226,-0.0742967091364493,
0.868149331745851));
#10917=CARTESIAN_POINT('Ctrl Pts',(-0.54708917182331,-0.115492077056649,
0.85981294420286));
#10918=CARTESIAN_POINT('Ctrl Pts',(-0.560922177770136,-0.141695629206859,
0.850993704737257));
#10919=CARTESIAN_POINT('Ctrl Pts',(-0.590422647829571,-0.181890537957859,
0.830754510485543));
#10920=CARTESIAN_POINT('Ctrl Pts',(-0.609616703125488,-0.201072148666545,
0.816896541396381));
#10921=CARTESIAN_POINT('Ctrl Pts',(-0.641117951819998,-0.223955109275652,
0.792310597819928));
#10922=CARTESIAN_POINT('Ctrl Pts',(-0.657208095763053,-0.232742381310829,
0.779109323683611));
#10923=CARTESIAN_POINT('Ctrl Pts',(-0.68964083160521,-0.244234834628584,
0.750552691816205));
#10924=CARTESIAN_POINT('Ctrl Pts',(-0.705971972091755,-0.246942143572133,
0.735185187071673));
#10925=CARTESIAN_POINT('Ctrl Pts',(-0.735185187071673,-0.246942143572133,
0.705971972091754));
#10926=CARTESIAN_POINT('Ctrl Pts',(-0.750552691816206,-0.244234834628584,
0.689640831605209));
#10927=CARTESIAN_POINT('Ctrl Pts',(-0.779109323683612,-0.232742381310829,
0.657208095763052));
#10928=CARTESIAN_POINT('Ctrl Pts',(-0.792310597819928,-0.223955109275652,
0.641117951819998));
#10929=CARTESIAN_POINT('Ctrl Pts',(-0.816896541396382,-0.201072148666545,
0.609616703125487));
#10930=CARTESIAN_POINT('Ctrl Pts',(-0.830754510485544,-0.181890537957858,
0.590422647829571));
#10931=CARTESIAN_POINT('Ctrl Pts',(-0.850993704737257,-0.141695629206858,
0.560922177770135));
#10932=CARTESIAN_POINT('Ctrl Pts',(-0.859812944202861,-0.115492077056649,
0.547089171823309));
#10933=CARTESIAN_POINT('Ctrl Pts',(-0.868149331745852,-0.0742967091364491,
0.533674141594226));
#10934=CARTESIAN_POINT('Ctrl Pts',(-0.870146645090731,-0.0609922781173483,
0.530395067942936));
#10935=CARTESIAN_POINT('Ctrl Pts',(-0.871530771444223,-0.04763,0.528110872004958));
#10936=CARTESIAN_POINT('',(-0.989696097314,-0.04763,0.242834539687906));
#10937=CARTESIAN_POINT('Origin',(0.,-0.04763,0.));
#10938=CARTESIAN_POINT('',(-1.019052,-0.246942143572133,1.248489836334E-16));
#10939=CARTESIAN_POINT('Ctrl Pts',(-0.989696097314,-0.04763,0.242834539687906));
#10940=CARTESIAN_POINT('Ctrl Pts',(-0.990332542620729,-0.0609922781173483,
0.24024064412003));
#10941=CARTESIAN_POINT('Ctrl Pts',(-0.991238884025248,-0.0742967091364492,
0.236509675094874));
#10942=CARTESIAN_POINT('Ctrl Pts',(-0.994830026707808,-0.115492077056649,
0.221129100087819));
#10943=CARTESIAN_POINT('Ctrl Pts',(-0.998375294985966,-0.141695629206859,
0.205111543747588));
#10944=CARTESIAN_POINT('Ctrl Pts',(-1.00492400591205,-0.181890537957859,
0.169940289819232));
#10945=CARTESIAN_POINT('Ctrl Pts',(-1.00869718865384,-0.201072148666545,
0.1465689792446));
#10946=CARTESIAN_POINT('Ctrl Pts',(-1.01358704779679,-0.223955109275652,
0.106909345252088));
#10947=CARTESIAN_POINT('Ctrl Pts',(-1.0156297872271,-0.232742381310829,
0.0861971848975944));
#10948=CARTESIAN_POINT('Ctrl Pts',(-1.01837060663223,-0.244234834628584,
0.0430711894098825));
#10949=CARTESIAN_POINT('Ctrl Pts',(-1.019052,-0.246942143572133,0.0206568624125608));
#10950=CARTESIAN_POINT('Ctrl Pts',(-1.019052,-0.246942143572133,1.2490009027033E-16));
#10951=CARTESIAN_POINT('',(-1.019052,-0.28578,1.24797876996471E-16));
#10952=CARTESIAN_POINT('',(-1.019052,-0.166705,1.24797876996471E-16));
#10953=CARTESIAN_POINT('Origin',(0.,-0.28578,0.));
#10954=CARTESIAN_POINT('',(-0.989696097314,-0.04763,-0.242834539687906));
#10955=CARTESIAN_POINT('Ctrl Pts',(-1.019052,-0.246942143572133,1.2490009027033E-16));
#10956=CARTESIAN_POINT('Ctrl Pts',(-1.019052,-0.246942143572133,-0.0206568624125605));
#10957=CARTESIAN_POINT('Ctrl Pts',(-1.01837060663223,-0.244234834628584,
-0.0430711894098822));
#10958=CARTESIAN_POINT('Ctrl Pts',(-1.0156297872271,-0.232742381310829,
-0.0861971848975941));
#10959=CARTESIAN_POINT('Ctrl Pts',(-1.01358704779679,-0.223955109275652,
-0.106909345252087));
#10960=CARTESIAN_POINT('Ctrl Pts',(-1.00869718865384,-0.201072148666546,
-0.1465689792446));
#10961=CARTESIAN_POINT('Ctrl Pts',(-1.00492400591205,-0.181890537957859,
-0.169940289819232));
#10962=CARTESIAN_POINT('Ctrl Pts',(-0.998375294985966,-0.141695629206859,
-0.205111543747588));
#10963=CARTESIAN_POINT('Ctrl Pts',(-0.994830026707808,-0.11549207705665,
-0.221129100087819));
#10964=CARTESIAN_POINT('Ctrl Pts',(-0.991238884025248,-0.0742967091364495,
-0.236509675094874));
#10965=CARTESIAN_POINT('Ctrl Pts',(-0.990332542620729,-0.0609922781173484,
-0.24024064412003));
#10966=CARTESIAN_POINT('Ctrl Pts',(-0.989696097314,-0.0476300000000001,
-0.242834539687907));
#10967=CARTESIAN_POINT('',(-0.871530771444223,-0.04763,-0.528110872004958));
#10968=CARTESIAN_POINT('Origin',(0.,-0.04763,0.));
#10969=CARTESIAN_POINT('',(-0.528110872004958,-0.04763,-0.871530771444223));
#10970=CARTESIAN_POINT('Ctrl Pts',(-0.871530771444223,-0.0476300000000001,
-0.528110872004958));
#10971=CARTESIAN_POINT('Ctrl Pts',(-0.87014664509073,-0.0609922781173484,
-0.530395067942936));
#10972=CARTESIAN_POINT('Ctrl Pts',(-0.868149331745851,-0.0742967091364494,
-0.533674141594226));
#10973=CARTESIAN_POINT('Ctrl Pts',(-0.85981294420286,-0.115492077056649,
-0.54708917182331));
#10974=CARTESIAN_POINT('Ctrl Pts',(-0.850993704737257,-0.141695629206859,
-0.560922177770136));
#10975=CARTESIAN_POINT('Ctrl Pts',(-0.830754510485543,-0.181890537957859,
-0.590422647829571));
#10976=CARTESIAN_POINT('Ctrl Pts',(-0.816896541396381,-0.201072148666546,
-0.609616703125488));
#10977=CARTESIAN_POINT('Ctrl Pts',(-0.792310597819928,-0.223955109275652,
-0.641117951819999));
#10978=CARTESIAN_POINT('Ctrl Pts',(-0.779109323683611,-0.232742381310829,
-0.657208095763053));
#10979=CARTESIAN_POINT('Ctrl Pts',(-0.750552691816205,-0.244234834628584,
-0.68964083160521));
#10980=CARTESIAN_POINT('Ctrl Pts',(-0.735185187071673,-0.246942143572133,
-0.705971972091755));
#10981=CARTESIAN_POINT('Ctrl Pts',(-0.705971972091754,-0.246942143572133,
-0.735185187071673));
#10982=CARTESIAN_POINT('Ctrl Pts',(-0.68964083160521,-0.244234834628584,
-0.750552691816206));
#10983=CARTESIAN_POINT('Ctrl Pts',(-0.657208095763052,-0.232742381310829,
-0.779109323683612));
#10984=CARTESIAN_POINT('Ctrl Pts',(-0.641117951819998,-0.223955109275652,
-0.792310597819928));
#10985=CARTESIAN_POINT('Ctrl Pts',(-0.609616703125488,-0.201072148666545,
-0.816896541396381));
#10986=CARTESIAN_POINT('Ctrl Pts',(-0.590422647829571,-0.181890537957859,
-0.830754510485543));
#10987=CARTESIAN_POINT('Ctrl Pts',(-0.560922177770136,-0.141695629206859,
-0.850993704737257));
#10988=CARTESIAN_POINT('Ctrl Pts',(-0.54708917182331,-0.115492077056649,
-0.85981294420286));
#10989=CARTESIAN_POINT('Ctrl Pts',(-0.533674141594226,-0.0742967091364494,
-0.868149331745852));
#10990=CARTESIAN_POINT('Ctrl Pts',(-0.530395067942936,-0.0609922781173484,
-0.870146645090731));
#10991=CARTESIAN_POINT('Ctrl Pts',(-0.528110872004958,-0.0476300000000001,
-0.871530771444223));
#10992=CARTESIAN_POINT('',(-0.242834539687906,-0.04763,-0.989696097314));
#10993=CARTESIAN_POINT('Origin',(0.,-0.04763,0.));
#10994=CARTESIAN_POINT('',(0.242834539687906,-0.04763,-0.989696097314));
#10995=CARTESIAN_POINT('Ctrl Pts',(-0.242834539687907,-0.04763,-0.989696097314));
#10996=CARTESIAN_POINT('Ctrl Pts',(-0.24024064412003,-0.0609922781173483,
-0.990332542620729));
#10997=CARTESIAN_POINT('Ctrl Pts',(-0.236509675094874,-0.0742967091364493,
-0.991238884025248));
#10998=CARTESIAN_POINT('Ctrl Pts',(-0.221129100087819,-0.115492077056649,
-0.994830026707808));
#10999=CARTESIAN_POINT('Ctrl Pts',(-0.205111543747588,-0.141695629206859,
-0.998375294985966));
#11000=CARTESIAN_POINT('Ctrl Pts',(-0.169940289819232,-0.181890537957859,
-1.00492400591205));
#11001=CARTESIAN_POINT('Ctrl Pts',(-0.1465689792446,-0.201072148666545,
-1.00869718865384));
#11002=CARTESIAN_POINT('Ctrl Pts',(-0.106909345252087,-0.223955109275652,
-1.01358704779679));
#11003=CARTESIAN_POINT('Ctrl Pts',(-0.0861971848975942,-0.232742381310829,
-1.0156297872271));
#11004=CARTESIAN_POINT('Ctrl Pts',(-0.0430711894098823,-0.244234834628584,
-1.01837060663223));
#11005=CARTESIAN_POINT('Ctrl Pts',(-0.0206568624125606,-0.246942143572133,
-1.019052));
#11006=CARTESIAN_POINT('Ctrl Pts',(0.0206568624125607,-0.246942143572133,
-1.019052));
#11007=CARTESIAN_POINT('Ctrl Pts',(0.0430711894098824,-0.244234834628584,
-1.01837060663223));
#11008=CARTESIAN_POINT('Ctrl Pts',(0.0861971848975943,-0.232742381310829,
-1.0156297872271));
#11009=CARTESIAN_POINT('Ctrl Pts',(0.106909345252088,-0.223955109275652,
-1.01358704779679));
#11010=CARTESIAN_POINT('Ctrl Pts',(0.1465689792446,-0.201072148666545,-1.00869718865384));
#11011=CARTESIAN_POINT('Ctrl Pts',(0.169940289819232,-0.181890537957859,
-1.00492400591205));
#11012=CARTESIAN_POINT('Ctrl Pts',(0.205111543747588,-0.141695629206859,
-0.998375294985966));
#11013=CARTESIAN_POINT('Ctrl Pts',(0.221129100087819,-0.115492077056649,
-0.994830026707808));
#11014=CARTESIAN_POINT('Ctrl Pts',(0.236509675094874,-0.0742967091364493,
-0.991238884025248));
#11015=CARTESIAN_POINT('Ctrl Pts',(0.24024064412003,-0.0609922781173484,
-0.990332542620729));
#11016=CARTESIAN_POINT('Ctrl Pts',(0.242834539687907,-0.04763,-0.989696097314));
#11017=CARTESIAN_POINT('',(0.528110872004958,-0.04763,-0.871530771444223));
#11018=CARTESIAN_POINT('Origin',(0.,-0.04763,0.));
#11019=CARTESIAN_POINT('',(0.871530771444223,-0.04763,-0.528110872004958));
#11020=CARTESIAN_POINT('Ctrl Pts',(0.528110872004958,-0.0476300000000001,
-0.871530771444223));
#11021=CARTESIAN_POINT('Ctrl Pts',(0.530395067942936,-0.0609922781173484,
-0.870146645090731));
#11022=CARTESIAN_POINT('Ctrl Pts',(0.533674141594226,-0.0742967091364493,
-0.868149331745851));
#11023=CARTESIAN_POINT('Ctrl Pts',(0.54708917182331,-0.115492077056649,
-0.85981294420286));
#11024=CARTESIAN_POINT('Ctrl Pts',(0.560922177770136,-0.141695629206859,
-0.850993704737257));
#11025=CARTESIAN_POINT('Ctrl Pts',(0.590422647829571,-0.181890537957859,
-0.830754510485543));
#11026=CARTESIAN_POINT('Ctrl Pts',(0.609616703125488,-0.201072148666545,
-0.816896541396381));
#11027=CARTESIAN_POINT('Ctrl Pts',(0.641117951819998,-0.223955109275652,
-0.792310597819928));
#11028=CARTESIAN_POINT('Ctrl Pts',(0.657208095763053,-0.232742381310829,
-0.779109323683612));
#11029=CARTESIAN_POINT('Ctrl Pts',(0.68964083160521,-0.244234834628584,
-0.750552691816206));
#11030=CARTESIAN_POINT('Ctrl Pts',(0.705971972091755,-0.246942143572133,
-0.735185187071673));
#11031=CARTESIAN_POINT('Ctrl Pts',(0.735185187071673,-0.246942143572133,
-0.705971972091754));
#11032=CARTESIAN_POINT('Ctrl Pts',(0.750552691816206,-0.244234834628584,
-0.68964083160521));
#11033=CARTESIAN_POINT('Ctrl Pts',(0.779109323683612,-0.232742381310829,
-0.657208095763053));
#11034=CARTESIAN_POINT('Ctrl Pts',(0.792310597819928,-0.223955109275652,
-0.641117951819998));
#11035=CARTESIAN_POINT('Ctrl Pts',(0.816896541396381,-0.201072148666545,
-0.609616703125488));
#11036=CARTESIAN_POINT('Ctrl Pts',(0.830754510485543,-0.181890537957859,
-0.590422647829571));
#11037=CARTESIAN_POINT('Ctrl Pts',(0.850993704737257,-0.141695629206859,
-0.560922177770136));
#11038=CARTESIAN_POINT('Ctrl Pts',(0.85981294420286,-0.115492077056649,
-0.54708917182331));
#11039=CARTESIAN_POINT('Ctrl Pts',(0.868149331745851,-0.0742967091364493,
-0.533674141594226));
#11040=CARTESIAN_POINT('Ctrl Pts',(0.870146645090731,-0.0609922781173484,
-0.530395067942936));
#11041=CARTESIAN_POINT('Ctrl Pts',(0.871530771444223,-0.0476300000000001,
-0.528110872004958));
#11042=CARTESIAN_POINT('',(0.989696097314,-0.04763,-0.242834539687906));
#11043=CARTESIAN_POINT('Origin',(0.,-0.04763,0.));
#11044=CARTESIAN_POINT('',(0.989696097314,-0.04763,0.242834539687906));
#11045=CARTESIAN_POINT('Ctrl Pts',(0.989696097314,-0.04763,-0.242834539687907));
#11046=CARTESIAN_POINT('Ctrl Pts',(0.990332542620729,-0.0609922781173483,
-0.24024064412003));
#11047=CARTESIAN_POINT('Ctrl Pts',(0.991238884025248,-0.0742967091364493,
-0.236509675094874));
#11048=CARTESIAN_POINT('Ctrl Pts',(0.994830026707808,-0.115492077056649,
-0.221129100087819));
#11049=CARTESIAN_POINT('Ctrl Pts',(0.998375294985966,-0.141695629206859,
-0.205111543747588));
#11050=CARTESIAN_POINT('Ctrl Pts',(1.00492400591205,-0.181890537957859,
-0.169940289819232));
#11051=CARTESIAN_POINT('Ctrl Pts',(1.00869718865384,-0.201072148666545,
-0.1465689792446));
#11052=CARTESIAN_POINT('Ctrl Pts',(1.01358704779679,-0.223955109275652,
-0.106909345252087));
#11053=CARTESIAN_POINT('Ctrl Pts',(1.0156297872271,-0.232742381310829,-0.0861971848975942));
#11054=CARTESIAN_POINT('Ctrl Pts',(1.01837060663223,-0.244234834628584,
-0.0430711894098823));
#11055=CARTESIAN_POINT('Ctrl Pts',(1.019052,-0.246942143572133,-0.0206568624125607));
#11056=CARTESIAN_POINT('Ctrl Pts',(1.019052,-0.246942143572133,0.0206568624125607));
#11057=CARTESIAN_POINT('Ctrl Pts',(1.01837060663223,-0.244234834628584,
0.0430711894098823));
#11058=CARTESIAN_POINT('Ctrl Pts',(1.0156297872271,-0.232742381310829,0.0861971848975942));
#11059=CARTESIAN_POINT('Ctrl Pts',(1.01358704779679,-0.223955109275652,
0.106909345252087));
#11060=CARTESIAN_POINT('Ctrl Pts',(1.00869718865384,-0.201072148666545,
0.1465689792446));
#11061=CARTESIAN_POINT('Ctrl Pts',(1.00492400591205,-0.181890537957859,
0.169940289819232));
#11062=CARTESIAN_POINT('Ctrl Pts',(0.998375294985966,-0.141695629206859,
0.205111543747588));
#11063=CARTESIAN_POINT('Ctrl Pts',(0.994830026707808,-0.115492077056649,
0.221129100087819));
#11064=CARTESIAN_POINT('Ctrl Pts',(0.991238884025248,-0.0742967091364492,
0.236509675094874));
#11065=CARTESIAN_POINT('Ctrl Pts',(0.990332542620729,-0.0609922781173483,
0.24024064412003));
#11066=CARTESIAN_POINT('Ctrl Pts',(0.989696097314,-0.04763,0.242834539687907));
#11067=CARTESIAN_POINT('Origin',(0.,-0.04763,0.));
#11068=CARTESIAN_POINT('Origin',(0.,-0.04763,0.));
#11069=CARTESIAN_POINT('',(0.238183666596899,-0.04763,0.951592097314));
#11070=CARTESIAN_POINT('Origin',(0.,-0.04763,0.));
#11071=CARTESIAN_POINT('Origin',(-1.94289029309402E-16,-0.04763,1.));
#11072=CARTESIAN_POINT('Origin',(-1.94289029309402E-16,0.,1.));
#11073=CARTESIAN_POINT('',(-0.2381836665969,-0.04763,0.951592097314));
#11074=CARTESIAN_POINT('Ctrl Pts',(-0.238183666596899,-0.0476299999999999,
0.951592097314));
#11075=CARTESIAN_POINT('Ctrl Pts',(-0.233157223576062,-0.0740444353928835,
0.952850216871763));
#11076=CARTESIAN_POINT('Ctrl Pts',(-0.223801617934946,-0.0999305678883309,
0.955173119738174));
#11077=CARTESIAN_POINT('Ctrl Pts',(-0.199966927975188,-0.142345102874864,
0.960411259488514));
#11078=CARTESIAN_POINT('Ctrl Pts',(-0.1868781821531,-0.159766064500479,
0.963103647174702));
#11079=CARTESIAN_POINT('Ctrl Pts',(-0.15681442133453,-0.190326085855194,
0.968453058988463));
#11080=CARTESIAN_POINT('Ctrl Pts',(-0.139836317888043,-0.203463743702801,
0.971100730005489));
#11081=CARTESIAN_POINT('Ctrl Pts',(-0.104422493053067,-0.224161999508995,
0.975530745318961));
#11082=CARTESIAN_POINT('Ctrl Pts',(-0.0842175114474176,-0.232861760990032,
0.977553872336861));
#11083=CARTESIAN_POINT('Ctrl Pts',(-0.0421062857595701,-0.244251601209411,
0.980270995488453));
#11084=CARTESIAN_POINT('Ctrl Pts',(-0.0201990724523197,-0.246942143572133,
0.980948));
#11085=CARTESIAN_POINT('Ctrl Pts',(0.020199072452319,-0.246942143572133,
0.980948));
#11086=CARTESIAN_POINT('Ctrl Pts',(0.0421062857595694,-0.244251601209411,
0.980270995488454));
#11087=CARTESIAN_POINT('Ctrl Pts',(0.0842175114474169,-0.232861760990032,
0.977553872336861));
#11088=CARTESIAN_POINT('Ctrl Pts',(0.104422493053067,-0.224161999508995,
0.975530745318961));
#11089=CARTESIAN_POINT('Ctrl Pts',(0.139836317888042,-0.203463743702801,
0.971100730005489));
#11090=CARTESIAN_POINT('Ctrl Pts',(0.15681442133453,-0.190326085855194,
0.968453058988463));
#11091=CARTESIAN_POINT('Ctrl Pts',(0.1868781821531,-0.15976606450048,0.963103647174702));
#11092=CARTESIAN_POINT('Ctrl Pts',(0.199966927975188,-0.142345102874864,
0.960411259488514));
#11093=CARTESIAN_POINT('Ctrl Pts',(0.223801617934945,-0.0999305678883309,
0.955173119738174));
#11094=CARTESIAN_POINT('Ctrl Pts',(0.233157223576061,-0.0740444353928835,
0.952850216871763));
#11095=CARTESIAN_POINT('Ctrl Pts',(0.238183666596899,-0.0476299999999999,
0.951592097314));
#11096=CARTESIAN_POINT('Origin',(-1.94289029309402E-16,-0.04763,1.));
#11097=CARTESIAN_POINT('Origin',(0.,-0.04763,0.));
#11098=CARTESIAN_POINT('',(-0.504455939115715,-0.04763,0.841298510752802));
#11099=CARTESIAN_POINT('Origin',(0.,-0.04763,0.));
#11100=CARTESIAN_POINT('Origin',(-0.707106781186548,-0.04763,0.707106781186547));
#11101=CARTESIAN_POINT('Origin',(-0.707106781186548,0.,0.707106781186547));
#11102=CARTESIAN_POINT('',(-0.841298510752802,-0.04763,0.504455939115715));
#11103=CARTESIAN_POINT('Ctrl Pts',(-0.841298510752802,-0.04763,0.504455939115715));
#11104=CARTESIAN_POINT('Ctrl Pts',(-0.838633903678357,-0.0740444353928835,
0.508899795931835));
#11105=CARTESIAN_POINT('Ctrl Pts',(-0.833661031856294,-0.0999305678883309,
0.517157748491652));
#11106=CARTESIAN_POINT('Ctrl Pts',(-0.820511285096538,-0.142345102874864,
0.537715343527944));
#11107=CARTESIAN_POINT('Ctrl Pts',(-0.813159949759,-0.159766064500479,0.548874290046456));
#11108=CARTESIAN_POINT('Ctrl Pts',(-0.795684265985089,-0.190326085855194,
0.573915184558107));
#11109=CARTESIAN_POINT('Ctrl Pts',(-0.78555112003688,-0.203463743702801,
0.587792702767295));
#11110=CARTESIAN_POINT('Ctrl Pts',(-0.763642258217233,-0.224161999508995,
0.615966552324775));
#11111=CARTESIAN_POINT('Ctrl Pts',(-0.750785745543687,-0.232861760990032,
0.631684198665438));
#11112=CARTESIAN_POINT('Ctrl Pts',(-0.722929908501543,-0.244251601209411,
0.663382628119203));
#11113=CARTESIAN_POINT('Ctrl Pts',(-0.707917883896095,-0.246942143572133,
0.679352081686668));
#11114=CARTESIAN_POINT('Ctrl Pts',(-0.679352081686668,-0.246942143572133,
0.707917883896095));
#11115=CARTESIAN_POINT('Ctrl Pts',(-0.663382628119203,-0.244251601209411,
0.722929908501544));
#11116=CARTESIAN_POINT('Ctrl Pts',(-0.631684198665438,-0.232861760990031,
0.750785745543687));
#11117=CARTESIAN_POINT('Ctrl Pts',(-0.615966552324775,-0.224161999508995,
0.763642258217233));
#11118=CARTESIAN_POINT('Ctrl Pts',(-0.587792702767295,-0.203463743702801,
0.78555112003688));
#11119=CARTESIAN_POINT('Ctrl Pts',(-0.573915184558107,-0.190326085855194,
0.795684265985088));
#11120=CARTESIAN_POINT('Ctrl Pts',(-0.548874290046456,-0.159766064500479,
0.813159949759));
#11121=CARTESIAN_POINT('Ctrl Pts',(-0.537715343527944,-0.142345102874864,
0.820511285096538));
#11122=CARTESIAN_POINT('Ctrl Pts',(-0.517157748491652,-0.0999305678883309,
0.833661031856294));
#11123=CARTESIAN_POINT('Ctrl Pts',(-0.508899795931835,-0.0740444353928835,
0.838633903678357));
#11124=CARTESIAN_POINT('Ctrl Pts',(-0.504455939115716,-0.04763,0.841298510752801));
#11125=CARTESIAN_POINT('Origin',(-0.707106781186548,-0.04763,0.707106781186547));
#11126=CARTESIAN_POINT('Origin',(0.,-0.04763,0.));
#11127=CARTESIAN_POINT('',(-0.951592097314,-0.04763,0.238183666596899));
#11128=CARTESIAN_POINT('Origin',(0.,-0.04763,0.));
#11129=CARTESIAN_POINT('Origin',(-1.,-0.04763,-1.11022302462516E-16));
#11130=CARTESIAN_POINT('Origin',(-1.,0.,-1.11022302462516E-16));
#11131=CARTESIAN_POINT('',(-0.951592097314,-0.04763,-0.2381836665969));
#11132=CARTESIAN_POINT('',(-0.980948,-0.246942143572133,1.08514323328844E-18));
#11133=CARTESIAN_POINT('Ctrl Pts',(-0.951592097314,-0.04763,-0.238183666596899));
#11134=CARTESIAN_POINT('Ctrl Pts',(-0.952850216871763,-0.0740444353928835,
-0.233157223576062));
#11135=CARTESIAN_POINT('Ctrl Pts',(-0.955173119738174,-0.0999305678883309,
-0.223801617934946));
#11136=CARTESIAN_POINT('Ctrl Pts',(-0.960411259488514,-0.142345102874864,
-0.199966927975188));
#11137=CARTESIAN_POINT('Ctrl Pts',(-0.963103647174702,-0.159766064500479,
-0.1868781821531));
#11138=CARTESIAN_POINT('Ctrl Pts',(-0.968453058988463,-0.190326085855194,
-0.15681442133453));
#11139=CARTESIAN_POINT('Ctrl Pts',(-0.971100730005489,-0.203463743702801,
-0.139836317888043));
#11140=CARTESIAN_POINT('Ctrl Pts',(-0.975530745318961,-0.224161999508995,
-0.104422493053067));
#11141=CARTESIAN_POINT('Ctrl Pts',(-0.977553872336861,-0.232861760990032,
-0.0842175114474175));
#11142=CARTESIAN_POINT('Ctrl Pts',(-0.980270995488453,-0.244251601209411,
-0.0421062857595699));
#11143=CARTESIAN_POINT('Ctrl Pts',(-0.980948,-0.246942143572133,-0.0201990724523195));
#11144=CARTESIAN_POINT('Ctrl Pts',(-0.980948,-0.246942143572133,-1.17961196366423E-16));
#11145=CARTESIAN_POINT('Origin',(-1.,-0.04763,-1.11022302462516E-16));
#11146=CARTESIAN_POINT('Ctrl Pts',(-0.980948,-0.246942143572133,-1.17961196366423E-16));
#11147=CARTESIAN_POINT('Ctrl Pts',(-0.980948,-0.246942143572133,0.0201990724523192));
#11148=CARTESIAN_POINT('Ctrl Pts',(-0.980270995488453,-0.244251601209411,
0.0421062857595695));
#11149=CARTESIAN_POINT('Ctrl Pts',(-0.977553872336861,-0.232861760990032,
0.0842175114474169));
#11150=CARTESIAN_POINT('Ctrl Pts',(-0.975530745318961,-0.224161999508995,
0.104422493053066));
#11151=CARTESIAN_POINT('Ctrl Pts',(-0.971100730005489,-0.203463743702801,
0.139836317888042));
#11152=CARTESIAN_POINT('Ctrl Pts',(-0.968453058988463,-0.190326085855194,
0.15681442133453));
#11153=CARTESIAN_POINT('Ctrl Pts',(-0.963103647174702,-0.15976606450048,
0.1868781821531));
#11154=CARTESIAN_POINT('Ctrl Pts',(-0.960411259488514,-0.142345102874864,
0.199966927975188));
#11155=CARTESIAN_POINT('Ctrl Pts',(-0.955173119738174,-0.099930567888331,
0.223801617934945));
#11156=CARTESIAN_POINT('Ctrl Pts',(-0.952850216871763,-0.0740444353928835,
0.233157223576061));
#11157=CARTESIAN_POINT('Ctrl Pts',(-0.951592097314,-0.04763,0.238183666596899));
#11158=CARTESIAN_POINT('Origin',(0.,-0.04763,0.));
#11159=CARTESIAN_POINT('',(-0.841298510752802,-0.04763,-0.504455939115715));
#11160=CARTESIAN_POINT('Origin',(0.,-0.04763,0.));
#11161=CARTESIAN_POINT('Origin',(-0.707106781186547,-0.04763,-0.707106781186548));
#11162=CARTESIAN_POINT('Origin',(-0.707106781186547,0.,-0.707106781186548));
#11163=CARTESIAN_POINT('',(-0.504455939115715,-0.04763,-0.841298510752802));
#11164=CARTESIAN_POINT('Ctrl Pts',(-0.504455939115715,-0.04763,-0.841298510752802));
#11165=CARTESIAN_POINT('Ctrl Pts',(-0.508899795931835,-0.0740444353928835,
-0.838633903678357));
#11166=CARTESIAN_POINT('Ctrl Pts',(-0.517157748491652,-0.0999305678883309,
-0.833661031856294));
#11167=CARTESIAN_POINT('Ctrl Pts',(-0.537715343527944,-0.142345102874864,
-0.820511285096538));
#11168=CARTESIAN_POINT('Ctrl Pts',(-0.548874290046456,-0.159766064500479,
-0.813159949759));
#11169=CARTESIAN_POINT('Ctrl Pts',(-0.573915184558107,-0.190326085855194,
-0.795684265985089));
#11170=CARTESIAN_POINT('Ctrl Pts',(-0.587792702767295,-0.203463743702801,
-0.78555112003688));
#11171=CARTESIAN_POINT('Ctrl Pts',(-0.615966552324775,-0.224161999508995,
-0.763642258217233));
#11172=CARTESIAN_POINT('Ctrl Pts',(-0.631684198665438,-0.232861760990032,
-0.750785745543687));
#11173=CARTESIAN_POINT('Ctrl Pts',(-0.663382628119203,-0.244251601209411,
-0.722929908501543));
#11174=CARTESIAN_POINT('Ctrl Pts',(-0.679352081686668,-0.246942143572133,
-0.707917883896095));
#11175=CARTESIAN_POINT('Ctrl Pts',(-0.707917883896095,-0.246942143572133,
-0.679352081686668));
#11176=CARTESIAN_POINT('Ctrl Pts',(-0.722929908501543,-0.244251601209411,
-0.663382628119203));
#11177=CARTESIAN_POINT('Ctrl Pts',(-0.750785745543687,-0.232861760990032,
-0.631684198665439));
#11178=CARTESIAN_POINT('Ctrl Pts',(-0.763642258217232,-0.224161999508995,
-0.615966552324775));
#11179=CARTESIAN_POINT('Ctrl Pts',(-0.78555112003688,-0.203463743702801,
-0.587792702767295));
#11180=CARTESIAN_POINT('Ctrl Pts',(-0.795684265985088,-0.190326085855194,
-0.573915184558107));
#11181=CARTESIAN_POINT('Ctrl Pts',(-0.813159949759,-0.15976606450048,-0.548874290046456));
#11182=CARTESIAN_POINT('Ctrl Pts',(-0.820511285096538,-0.142345102874864,
-0.537715343527944));
#11183=CARTESIAN_POINT('Ctrl Pts',(-0.833661031856294,-0.0999305678883311,
-0.517157748491652));
#11184=CARTESIAN_POINT('Ctrl Pts',(-0.838633903678357,-0.0740444353928836,
-0.508899795931835));
#11185=CARTESIAN_POINT('Ctrl Pts',(-0.841298510752801,-0.04763,-0.504455939115715));
#11186=CARTESIAN_POINT('Origin',(-0.707106781186547,-0.04763,-0.707106781186548));
#11187=CARTESIAN_POINT('Origin',(0.,-0.04763,0.));
#11188=CARTESIAN_POINT('',(-0.238183666596899,-0.04763,-0.951592097314));
#11189=CARTESIAN_POINT('Origin',(0.,-0.04763,0.));
#11190=CARTESIAN_POINT('Origin',(5.55111512312578E-17,-0.04763,-1.));
#11191=CARTESIAN_POINT('Origin',(5.55111512312578E-17,0.,-1.));
#11192=CARTESIAN_POINT('',(0.238183666596899,-0.04763,-0.951592097314));
#11193=CARTESIAN_POINT('Ctrl Pts',(0.238183666596899,-0.04763,-0.951592097314));
#11194=CARTESIAN_POINT('Ctrl Pts',(0.233157223576062,-0.0740444353928835,
-0.952850216871763));
#11195=CARTESIAN_POINT('Ctrl Pts',(0.223801617934946,-0.099930567888331,
-0.955173119738174));
#11196=CARTESIAN_POINT('Ctrl Pts',(0.199966927975188,-0.142345102874864,
-0.960411259488514));
#11197=CARTESIAN_POINT('Ctrl Pts',(0.1868781821531,-0.15976606450048,-0.963103647174702));
#11198=CARTESIAN_POINT('Ctrl Pts',(0.15681442133453,-0.190326085855194,
-0.968453058988463));
#11199=CARTESIAN_POINT('Ctrl Pts',(0.139836317888042,-0.203463743702801,
-0.971100730005489));
#11200=CARTESIAN_POINT('Ctrl Pts',(0.104422493053067,-0.224161999508995,
-0.975530745318961));
#11201=CARTESIAN_POINT('Ctrl Pts',(0.0842175114474173,-0.232861760990032,
-0.977553872336861));
#11202=CARTESIAN_POINT('Ctrl Pts',(0.0421062857595698,-0.244251601209411,
-0.980270995488453));
#11203=CARTESIAN_POINT('Ctrl Pts',(0.0201990724523194,-0.246942143572133,
-0.980948));
#11204=CARTESIAN_POINT('Ctrl Pts',(-0.0201990724523193,-0.246942143572133,
-0.980948));
#11205=CARTESIAN_POINT('Ctrl Pts',(-0.0421062857595697,-0.244251601209411,
-0.980270995488453));
#11206=CARTESIAN_POINT('Ctrl Pts',(-0.0842175114474171,-0.232861760990032,
-0.977553872336861));
#11207=CARTESIAN_POINT('Ctrl Pts',(-0.104422493053067,-0.224161999508995,
-0.975530745318961));
#11208=CARTESIAN_POINT('Ctrl Pts',(-0.139836317888042,-0.203463743702801,
-0.971100730005489));
#11209=CARTESIAN_POINT('Ctrl Pts',(-0.15681442133453,-0.190326085855194,
-0.968453058988463));
#11210=CARTESIAN_POINT('Ctrl Pts',(-0.1868781821531,-0.15976606450048,-0.963103647174702));
#11211=CARTESIAN_POINT('Ctrl Pts',(-0.199966927975188,-0.142345102874864,
-0.960411259488514));
#11212=CARTESIAN_POINT('Ctrl Pts',(-0.223801617934945,-0.099930567888331,
-0.955173119738174));
#11213=CARTESIAN_POINT('Ctrl Pts',(-0.233157223576062,-0.0740444353928835,
-0.952850216871763));
#11214=CARTESIAN_POINT('Ctrl Pts',(-0.238183666596899,-0.0476299999999999,
-0.951592097314));
#11215=CARTESIAN_POINT('Origin',(5.55111512312578E-17,-0.04763,-1.));
#11216=CARTESIAN_POINT('Origin',(0.,-0.04763,0.));
#11217=CARTESIAN_POINT('',(0.504455939115715,-0.04763,-0.841298510752802));
#11218=CARTESIAN_POINT('Origin',(0.,-0.04763,0.));
#11219=CARTESIAN_POINT('Origin',(0.707106781186548,-0.04763,-0.707106781186547));
#11220=CARTESIAN_POINT('Origin',(0.707106781186548,0.,-0.707106781186547));
#11221=CARTESIAN_POINT('',(0.841298510752802,-0.04763,-0.504455939115715));
#11222=CARTESIAN_POINT('Ctrl Pts',(0.841298510752802,-0.04763,-0.504455939115715));
#11223=CARTESIAN_POINT('Ctrl Pts',(0.838633903678357,-0.0740444353928835,
-0.508899795931835));
#11224=CARTESIAN_POINT('Ctrl Pts',(0.833661031856294,-0.0999305678883309,
-0.517157748491652));
#11225=CARTESIAN_POINT('Ctrl Pts',(0.820511285096538,-0.142345102874864,
-0.537715343527944));
#11226=CARTESIAN_POINT('Ctrl Pts',(0.813159949759,-0.159766064500479,-0.548874290046456));
#11227=CARTESIAN_POINT('Ctrl Pts',(0.795684265985088,-0.190326085855194,
-0.573915184558107));
#11228=CARTESIAN_POINT('Ctrl Pts',(0.78555112003688,-0.203463743702801,
-0.587792702767295));
#11229=CARTESIAN_POINT('Ctrl Pts',(0.763642258217233,-0.224161999508995,
-0.615966552324775));
#11230=CARTESIAN_POINT('Ctrl Pts',(0.750785745543687,-0.232861760990032,
-0.631684198665438));
#11231=CARTESIAN_POINT('Ctrl Pts',(0.722929908501543,-0.244251601209411,
-0.663382628119203));
#11232=CARTESIAN_POINT('Ctrl Pts',(0.707917883896095,-0.246942143572133,
-0.679352081686668));
#11233=CARTESIAN_POINT('Ctrl Pts',(0.679352081686668,-0.246942143572133,
-0.707917883896095));
#11234=CARTESIAN_POINT('Ctrl Pts',(0.663382628119203,-0.244251601209411,
-0.722929908501543));
#11235=CARTESIAN_POINT('Ctrl Pts',(0.631684198665438,-0.232861760990032,
-0.750785745543687));
#11236=CARTESIAN_POINT('Ctrl Pts',(0.615966552324775,-0.224161999508995,
-0.763642258217232));
#11237=CARTESIAN_POINT('Ctrl Pts',(0.587792702767295,-0.203463743702801,
-0.78555112003688));
#11238=CARTESIAN_POINT('Ctrl Pts',(0.573915184558107,-0.190326085855194,
-0.795684265985088));
#11239=CARTESIAN_POINT('Ctrl Pts',(0.548874290046456,-0.159766064500479,
-0.813159949759));
#11240=CARTESIAN_POINT('Ctrl Pts',(0.537715343527944,-0.142345102874864,
-0.820511285096538));
#11241=CARTESIAN_POINT('Ctrl Pts',(0.517157748491652,-0.099930567888331,
-0.833661031856294));
#11242=CARTESIAN_POINT('Ctrl Pts',(0.508899795931835,-0.0740444353928835,
-0.838633903678357));
#11243=CARTESIAN_POINT('Ctrl Pts',(0.504455939115715,-0.04763,-0.841298510752801));
#11244=CARTESIAN_POINT('Origin',(0.707106781186548,-0.04763,-0.707106781186547));
#11245=CARTESIAN_POINT('Origin',(0.,-0.166705,0.));
#11246=CARTESIAN_POINT('',(-0.980948,-0.28578,1.20131482833E-16));
#11247=CARTESIAN_POINT('Origin',(0.,-0.28578,0.));
#11248=CARTESIAN_POINT('',(-0.980948,-0.166705,1.20131482833E-16));
#11249=CARTESIAN_POINT('',(0.951592097314,-0.04763,0.238183666596899));
#11250=CARTESIAN_POINT('Origin',(0.,-0.04763,0.));
#11251=CARTESIAN_POINT('',(0.951592097314,-0.04763,-0.238183666596899));
#11252=CARTESIAN_POINT('Ctrl Pts',(0.951592097314,-0.04763,0.238183666596899));
#11253=CARTESIAN_POINT('Ctrl Pts',(0.952850216871763,-0.0740444353928835,
0.233157223576062));
#11254=CARTESIAN_POINT('Ctrl Pts',(0.955173119738174,-0.099930567888331,
0.223801617934945));
#11255=CARTESIAN_POINT('Ctrl Pts',(0.960411259488514,-0.142345102874864,
0.199966927975188));
#11256=CARTESIAN_POINT('Ctrl Pts',(0.963103647174702,-0.15976606450048,
0.1868781821531));
#11257=CARTESIAN_POINT('Ctrl Pts',(0.968453058988463,-0.190326085855194,
0.15681442133453));
#11258=CARTESIAN_POINT('Ctrl Pts',(0.971100730005489,-0.203463743702801,
0.139836317888042));
#11259=CARTESIAN_POINT('Ctrl Pts',(0.975530745318961,-0.224161999508995,
0.104422493053067));
#11260=CARTESIAN_POINT('Ctrl Pts',(0.977553872336861,-0.232861760990032,
0.0842175114474172));
#11261=CARTESIAN_POINT('Ctrl Pts',(0.980270995488453,-0.244251601209411,
0.0421062857595697));
#11262=CARTESIAN_POINT('Ctrl Pts',(0.980948,-0.246942143572133,0.0201990724523194));
#11263=CARTESIAN_POINT('Ctrl Pts',(0.980948,-0.246942143572133,-0.0201990724523194));
#11264=CARTESIAN_POINT('Ctrl Pts',(0.980270995488453,-0.244251601209411,
-0.0421062857595697));
#11265=CARTESIAN_POINT('Ctrl Pts',(0.977553872336861,-0.232861760990032,
-0.0842175114474172));
#11266=CARTESIAN_POINT('Ctrl Pts',(0.975530745318961,-0.224161999508995,
-0.104422493053067));
#11267=CARTESIAN_POINT('Ctrl Pts',(0.971100730005489,-0.203463743702801,
-0.139836317888042));
#11268=CARTESIAN_POINT('Ctrl Pts',(0.968453058988463,-0.190326085855194,
-0.15681442133453));
#11269=CARTESIAN_POINT('Ctrl Pts',(0.963103647174702,-0.15976606450048,
-0.1868781821531));
#11270=CARTESIAN_POINT('Ctrl Pts',(0.960411259488514,-0.142345102874864,
-0.199966927975188));
#11271=CARTESIAN_POINT('Ctrl Pts',(0.955173119738174,-0.099930567888331,
-0.223801617934945));
#11272=CARTESIAN_POINT('Ctrl Pts',(0.952850216871763,-0.0740444353928835,
-0.233157223576062));
#11273=CARTESIAN_POINT('Ctrl Pts',(0.951592097314,-0.0476299999999999,-0.238183666596899));
#11274=CARTESIAN_POINT('Origin',(0.,-0.04763,0.));
#11275=CARTESIAN_POINT('Origin',(0.,-0.04763,0.));
#11276=CARTESIAN_POINT('Origin',(1.,-0.04763,0.));
#11277=CARTESIAN_POINT('Origin',(1.,0.,0.));
#11278=CARTESIAN_POINT('Origin',(1.,-0.04763,0.));
#11279=CARTESIAN_POINT('Origin',(0.,-0.28578,0.));
#11280=CARTESIAN_POINT('Origin',(0.,-0.04763,0.));
#11281=CARTESIAN_POINT('',(0.,0.,0.));
#11282=CARTESIAN_POINT('Origin',(1.013815,0.445,0.));
#11283=CARTESIAN_POINT('',(-1.013815,0.445,-1.24156529467757E-16));
#11284=CARTESIAN_POINT('Origin',(0.,0.445,0.));
#11285=CARTESIAN_POINT('',(-0.991185,0.445,-1.21385153761287E-16));
#11286=CARTESIAN_POINT('Origin',(0.,0.445,0.));
#11287=CARTESIAN_POINT('Origin',(0.,0.4075,0.));
#11288=CARTESIAN_POINT('',(-1.013815,0.37,-1.24156529467757E-16));
#11289=CARTESIAN_POINT('Origin',(0.,0.37,0.));
#11290=CARTESIAN_POINT('',(-1.013815,0.4075,-1.24156529467757E-16));
#11291=CARTESIAN_POINT('Origin',(0.991185,0.37,0.));
#11292=CARTESIAN_POINT('',(-0.991185,0.37,-1.21385153761287E-16));
#11293=CARTESIAN_POINT('Origin',(0.,0.37,0.));
#11294=CARTESIAN_POINT('Origin',(0.,0.4075,0.));
#11295=CARTESIAN_POINT('',(-0.991185,0.4075,-1.21385153761287E-16));
#11296=CARTESIAN_POINT('Origin',(1.013815,-0.37,0.));
#11297=CARTESIAN_POINT('',(-1.013815,-0.37,-1.24156529467757E-16));
#11298=CARTESIAN_POINT('Origin',(0.,-0.37,0.));
#11299=CARTESIAN_POINT('',(-0.991185,-0.37,-1.21385153761287E-16));
#11300=CARTESIAN_POINT('Origin',(0.,-0.37,0.));
#11301=CARTESIAN_POINT('Origin',(0.,-0.4075,0.));
#11302=CARTESIAN_POINT('',(-1.013815,-0.445,-1.24156529467757E-16));
#11303=CARTESIAN_POINT('Origin',(0.,-0.445,0.));
#11304=CARTESIAN_POINT('',(-1.013815,-0.4075,-1.24156529467757E-16));
#11305=CARTESIAN_POINT('Origin',(0.991185,-0.445,0.));
#11306=CARTESIAN_POINT('',(-0.991185,-0.445,-1.21385153761287E-16));
#11307=CARTESIAN_POINT('Origin',(0.,-0.445,0.));
#11308=CARTESIAN_POINT('Origin',(0.,-0.4075,0.));
#11309=CARTESIAN_POINT('',(-0.991185,-0.4075,-1.21385153761287E-16));
#11310=CARTESIAN_POINT('',(0.,0.,0.));
#11311=CARTESIAN_POINT('',(0.,0.,0.));
#11312=CARTESIAN_POINT('',(0.,0.,0.));
#11313=CARTESIAN_POINT('',(0.,0.,0.));
#11314=CARTESIAN_POINT('',(0.,0.,0.));
#11315=CARTESIAN_POINT('',(0.,0.,0.));
#11316=CARTESIAN_POINT('',(0.,0.,0.));
#11317=CARTESIAN_POINT('Origin',(0.75,1.2,0.));
#11318=CARTESIAN_POINT('',(0.885663593019381,1.2,-0.16));
#11319=CARTESIAN_POINT('',(0.885663593019381,1.2,0.16));
#11320=CARTESIAN_POINT('Origin',(0.,1.2,0.));
#11321=CARTESIAN_POINT('',(0.93,1.2,-0.16));
#11322=CARTESIAN_POINT('',(0.93,1.2,-0.16));
#11323=CARTESIAN_POINT('',(0.93,1.2,0.16));
#11324=CARTESIAN_POINT('',(0.93,1.2,0.16));
#11325=CARTESIAN_POINT('',(0.57,1.2,0.16));
#11326=CARTESIAN_POINT('Origin',(0.57,0.,0.16));
#11327=CARTESIAN_POINT('',(0.885663593019381,-1.2,0.16));
#11328=CARTESIAN_POINT('',(0.885663593019381,0.,0.16));
#11329=CARTESIAN_POINT('',(0.93,-1.2,0.16));
#11330=CARTESIAN_POINT('',(0.93,0.,0.16));
#11331=CARTESIAN_POINT('',(0.57,-1.2,0.16));
#11332=CARTESIAN_POINT('Origin',(0.75,-1.2,0.));
#11333=CARTESIAN_POINT('',(0.885663593019381,-1.2,-0.16));
#11334=CARTESIAN_POINT('Origin',(0.,-1.2,0.));
#11335=CARTESIAN_POINT('',(0.93,-1.2,-0.16));
#11336=CARTESIAN_POINT('',(0.93,-1.2,0.16));
#11337=CARTESIAN_POINT('',(0.93,-1.2,-0.16));
#11338=CARTESIAN_POINT('Origin',(0.93,0.,-0.16));
#11339=CARTESIAN_POINT('',(0.885663593019381,0.,-0.16));
#11340=CARTESIAN_POINT('',(0.93,0.,-0.16));
#11341=CARTESIAN_POINT('Origin',(0.93,0.,0.16));
#11342=CARTESIAN_POINT('Origin',(1.05,1.5,0.));
#11343=CARTESIAN_POINT('',(-1.05,1.5,-1.28587913910472E-16));
#11344=CARTESIAN_POINT('Origin',(0.,1.5,0.));
#11345=CARTESIAN_POINT('',(-0.9,1.5,-1.10218211923262E-16));
#11346=CARTESIAN_POINT('Origin',(0.,1.5,0.));
#11347=CARTESIAN_POINT('Origin',(0.,1.315,0.));
#11348=CARTESIAN_POINT('',(-1.05,1.13,-1.28587913910472E-16));
#11349=CARTESIAN_POINT('Origin',(0.,1.13,0.));
#11350=CARTESIAN_POINT('',(-1.05,1.315,-1.28587913910472E-16));
#11351=CARTESIAN_POINT('Origin',(1.,1.13,0.));
#11352=CARTESIAN_POINT('',(-1.,1.13,-1.22464679914735E-16));
#11353=CARTESIAN_POINT('Origin',(0.,1.13,0.));
#11354=CARTESIAN_POINT('Origin',(0.,1.065,0.));
#11355=CARTESIAN_POINT('',(-1.,1.,-1.22464679914735E-16));
#11356=CARTESIAN_POINT('Origin',(0.,1.,0.));
#11357=CARTESIAN_POINT('',(-1.,1.065,-1.22464679914735E-16));
#11358=CARTESIAN_POINT('Origin',(1.05,1.,0.));
#11359=CARTESIAN_POINT('',(-1.05,1.,-1.28587913910472E-16));
#11360=CARTESIAN_POINT('Origin',(0.,1.,0.));
#11361=CARTESIAN_POINT('Origin',(0.,0.,0.));
#11362=CARTESIAN_POINT('',(-1.05,-1.,-1.28587913910472E-16));
#11363=CARTESIAN_POINT('Origin',(0.,-1.,0.));
#11364=CARTESIAN_POINT('',(-1.05,0.,-1.28587913910472E-16));
#11365=CARTESIAN_POINT('Origin',(1.,-1.,0.));
#11366=CARTESIAN_POINT('',(-1.,-1.,-1.22464679914735E-16));
#11367=CARTESIAN_POINT('Origin',(0.,-1.,0.));
#11368=CARTESIAN_POINT('Origin',(0.,-1.065,0.));
#11369=CARTESIAN_POINT('',(-1.,-1.13,-1.22464679914735E-16));
#11370=CARTESIAN_POINT('Origin',(0.,-1.13,0.));
#11371=CARTESIAN_POINT('',(-1.,-1.065,-1.22464679914735E-16));
#11372=CARTESIAN_POINT('Origin',(1.05,-1.13,0.));
#11373=CARTESIAN_POINT('',(-1.05,-1.13,-1.28587913910472E-16));
#11374=CARTESIAN_POINT('Origin',(0.,-1.13,0.));
#11375=CARTESIAN_POINT('Origin',(0.,-1.315,0.));
#11376=CARTESIAN_POINT('',(-1.05,-1.5,-1.28587913910472E-16));
#11377=CARTESIAN_POINT('Origin',(0.,-1.5,0.));
#11378=CARTESIAN_POINT('',(-1.05,-1.315,-1.28587913910472E-16));
#11379=CARTESIAN_POINT('Origin',(0.9,-1.5,0.));
#11380=CARTESIAN_POINT('',(-0.9,-1.5,-1.10218211923262E-16));
#11381=CARTESIAN_POINT('Origin',(0.,-1.5,0.));
#11382=CARTESIAN_POINT('Origin',(0.,0.,0.));
#11383=CARTESIAN_POINT('',(-0.9,0.,-1.10218211923262E-16));
#11384=CARTESIAN_POINT('',(0.,0.,0.));
#11385=CARTESIAN_POINT('Origin',(0.75,1.2,0.));
#11386=CARTESIAN_POINT('',(0.880582193778639,1.2,0.16));
#11387=CARTESIAN_POINT('',(0.880582193778639,1.2,-0.16));
#11388=CARTESIAN_POINT('Origin',(0.,1.2,0.));
#11389=CARTESIAN_POINT('',(0.583459510163302,1.2,0.16));
#11390=CARTESIAN_POINT('',(0.57,1.2,0.16));
#11391=CARTESIAN_POINT('',(0.583459510163302,1.2,-0.16));
#11392=CARTESIAN_POINT('Origin',(0.,1.2,0.));
#11393=CARTESIAN_POINT('',(0.93,1.2,-0.16));
#11394=CARTESIAN_POINT('Origin',(0.93,0.,-0.16));
#11395=CARTESIAN_POINT('',(0.880582193778639,-1.2,-0.16));
#11396=CARTESIAN_POINT('',(0.880582193778639,0.,-0.16));
#11397=CARTESIAN_POINT('',(0.583459510163302,-1.2,-0.16));
#11398=CARTESIAN_POINT('',(0.583459510163302,0.,-0.16));
#11399=CARTESIAN_POINT('',(0.93,-1.2,-0.16));
#11400=CARTESIAN_POINT('Origin',(0.75,-1.2,0.));
#11401=CARTESIAN_POINT('',(0.880582193778639,-1.2,0.16));
#11402=CARTESIAN_POINT('Origin',(0.,-1.2,0.));
#11403=CARTESIAN_POINT('',(0.583459510163302,-1.2,0.16));
#11404=CARTESIAN_POINT('Origin',(0.,-1.2,0.));
#11405=CARTESIAN_POINT('',(0.57,-1.2,0.16));
#11406=CARTESIAN_POINT('Origin',(0.57,0.,0.16));
#11407=CARTESIAN_POINT('',(0.880582193778639,0.,0.16));
#11408=CARTESIAN_POINT('',(0.583459510163302,0.,0.16));
#11409=CARTESIAN_POINT('Origin',(0.895,1.35,0.));
#11410=CARTESIAN_POINT('',(-0.895,1.35,-1.09605888523688E-16));
#11411=CARTESIAN_POINT('Origin',(0.,1.35,0.));
#11412=CARTESIAN_POINT('',(-0.605,1.35,-7.40911313484149E-17));
#11413=CARTESIAN_POINT('Origin',(0.,1.35,0.));
#11414=CARTESIAN_POINT('Origin',(0.,0.,0.));
#11415=CARTESIAN_POINT('',(-0.895,-1.35,-1.09605888523688E-16));
#11416=CARTESIAN_POINT('Origin',(0.,-1.35,0.));
#11417=CARTESIAN_POINT('',(-0.895,0.,-1.09605888523688E-16));
#11418=CARTESIAN_POINT('Origin',(0.605,-1.35,0.));
#11419=CARTESIAN_POINT('',(-0.605,-1.35,-7.40911313484149E-17));
#11420=CARTESIAN_POINT('Origin',(0.,-1.35,0.));
#11421=CARTESIAN_POINT('Origin',(0.,0.,0.));
#11422=CARTESIAN_POINT('',(-0.605,0.,-7.40911313484149E-17));
#11423=CARTESIAN_POINT('',(0.,0.,0.));
#11424=CARTESIAN_POINT('',(0.,0.,0.));
#11425=CARTESIAN_POINT('',(0.,0.,0.));
#11426=CARTESIAN_POINT('Origin',(0.0866025403784439,-0.4,-0.15));
#11427=CARTESIAN_POINT('',(0.173205080756888,-0.4,0.));
#11428=CARTESIAN_POINT('',(0.0866025403784439,-0.4,-0.15));
#11429=CARTESIAN_POINT('',(0.173205080756888,-0.4,0.));
#11430=CARTESIAN_POINT('',(0.0866025403784439,-0.64,-0.15));
#11431=CARTESIAN_POINT('',(0.0866025403784439,-0.4,-0.15));
#11432=CARTESIAN_POINT('',(0.173205080756888,-0.64,0.));
#11433=CARTESIAN_POINT('',(0.173205080756888,-0.64,0.));
#11434=CARTESIAN_POINT('',(0.173205080756888,-0.4,0.));
#11435=CARTESIAN_POINT('Origin',(-0.0866025403784438,-0.4,-0.15));
#11436=CARTESIAN_POINT('',(-0.0866025403784438,-0.4,-0.15));
#11437=CARTESIAN_POINT('',(0.0866025403784439,-0.4,-0.15));
#11438=CARTESIAN_POINT('',(-0.0866025403784438,-0.64,-0.15));
#11439=CARTESIAN_POINT('',(-0.0866025403784438,-0.4,-0.15));
#11440=CARTESIAN_POINT('',(0.0866025403784439,-0.64,-0.15));
#11441=CARTESIAN_POINT('Origin',(-0.173205080756888,-0.4,-2.77555756156289E-17));
#11442=CARTESIAN_POINT('',(-0.173205080756888,-0.4,-2.12115047744981E-17));
#11443=CARTESIAN_POINT('',(-0.0866025403784438,-0.4,-0.15));
#11444=CARTESIAN_POINT('',(-0.173205080756888,-0.64,-2.77555756156289E-17));
#11445=CARTESIAN_POINT('',(-0.173205080756888,-0.4,-2.12115047744981E-17));
#11446=CARTESIAN_POINT('',(-0.0866025403784438,-0.64,-0.15));
#11447=CARTESIAN_POINT('Origin',(-0.0866025403784439,-0.4,0.15));
#11448=CARTESIAN_POINT('',(-0.0866025403784439,-0.4,0.15));
#11449=CARTESIAN_POINT('',(-0.173205080756888,-0.4,-2.12115047744981E-17));
#11450=CARTESIAN_POINT('',(-0.0866025403784439,-0.64,0.15));
#11451=CARTESIAN_POINT('',(-0.0866025403784439,-0.4,0.15));
#11452=CARTESIAN_POINT('',(-0.173205080756888,-0.64,-2.12115047744981E-17));
#11453=CARTESIAN_POINT('Origin',(0.0866025403784439,-0.4,0.15));
#11454=CARTESIAN_POINT('',(0.0866025403784439,-0.4,0.15));
#11455=CARTESIAN_POINT('',(-0.0866025403784439,-0.4,0.15));
#11456=CARTESIAN_POINT('',(0.0866025403784439,-0.64,0.15));
#11457=CARTESIAN_POINT('',(0.0866025403784439,-0.4,0.15));
#11458=CARTESIAN_POINT('',(-0.0866025403784439,-0.64,0.15));
#11459=CARTESIAN_POINT('Origin',(0.173205080756888,-0.4,0.));
#11460=CARTESIAN_POINT('',(0.0866025403784439,-0.4,0.15));
#11461=CARTESIAN_POINT('',(0.0866025403784439,-0.64,0.15));
#11462=CARTESIAN_POINT('Origin',(0.,-0.4,-2.77555756156289E-17));
#11463=CARTESIAN_POINT('Origin',(0.,-0.64,-2.77555756156289E-17));
#11464=CARTESIAN_POINT('Origin',(0.,-1.6,0.));
#11465=CARTESIAN_POINT('',(-0.2,-1.6,2.44929359829471E-17));
#11466=CARTESIAN_POINT('Origin',(0.,-1.6,0.));
#11467=CARTESIAN_POINT('',(-0.16,-1.6,-1.95943487863577E-17));
#11468=CARTESIAN_POINT('Origin',(0.,-1.6,0.));
#11469=CARTESIAN_POINT('Origin',(0.,-3.,0.));
#11470=CARTESIAN_POINT('',(-0.2,-3.,2.44929359829471E-17));
#11471=CARTESIAN_POINT('',(-0.2,-3.,2.44929359829471E-17));
#11472=CARTESIAN_POINT('Origin',(0.,-3.,0.));
#11473=CARTESIAN_POINT('Origin',(0.,-3.,0.));
#11474=CARTESIAN_POINT('Origin',(0.3,0.4,0.));
#11475=CARTESIAN_POINT('',(-0.3,0.4,-3.67394039744206E-17));
#11476=CARTESIAN_POINT('Origin',(0.,0.4,0.));
#11477=CARTESIAN_POINT('Origin',(0.,0.375,0.));
#11478=CARTESIAN_POINT('',(-0.35,0.35,-4.28626379701573E-17));
#11479=CARTESIAN_POINT('Origin',(0.,0.35,0.));
#11480=CARTESIAN_POINT('',(-0.325,0.375,-3.9801020972289E-17));
#11481=CARTESIAN_POINT('Origin',(0.,0.19,0.));
#11482=CARTESIAN_POINT('',(-0.35,0.03,-4.28626379701574E-17));
#11483=CARTESIAN_POINT('Origin',(0.,0.03,0.));
#11484=CARTESIAN_POINT('',(-0.35,0.19,-4.28626379701574E-17));
#11485=CARTESIAN_POINT('Origin',(0.,0.0149999999999999,0.));
#11486=CARTESIAN_POINT('',(-0.32,-3.29597460435593E-17,-3.91886975727153E-17));
#11487=CARTESIAN_POINT('Origin',(0.,0.,0.));
#11488=CARTESIAN_POINT('',(-0.335,0.0149999999999999,-4.10256677714363E-17));
#11489=CARTESIAN_POINT('Origin',(0.22,0.,0.));
#11490=CARTESIAN_POINT('',(-0.22,-6.93889390390723E-18,-2.69422295812418E-17));
#11491=CARTESIAN_POINT('Origin',(0.,0.,0.));
#11492=CARTESIAN_POINT('Origin',(0.,-0.02,0.));
#11493=CARTESIAN_POINT('',(-0.1954,-0.0492,2.39295984553393E-17));
#11494=CARTESIAN_POINT('Origin',(0.,-0.0492,0.));
#11495=CARTESIAN_POINT('',(-0.21,-0.02,-2.57175827820944E-17));
#11496=CARTESIAN_POINT('Origin',(0.,-0.8,0.));
#11497=CARTESIAN_POINT('',(-0.1954,-1.5646,2.39295984553393E-17));
#11498=CARTESIAN_POINT('Origin',(0.,-1.5646,0.));
#11499=CARTESIAN_POINT('',(-0.1954,-0.8,-2.39295984553393E-17));
#11500=CARTESIAN_POINT('Origin',(0.,-1.58,0.));
#11501=CARTESIAN_POINT('',(-0.18,-1.58,-2.20436423846524E-17));
#11502=CARTESIAN_POINT('',(0.,0.,0.));
#11503=CARTESIAN_POINT('',(0.,0.,0.));
#11504=CARTESIAN_POINT('Origin',(-2.82632109303527,-3.6,8.79263101785268));
#11505=CARTESIAN_POINT('',(-3.13132109303527,-3.5,8.79263101785268));
#11506=CARTESIAN_POINT('Origin',(-2.82632109303527,-3.5,8.79263101785268));
#11507=CARTESIAN_POINT('',(-3.13132109303527,-2.7,8.79263101785268));
#11508=CARTESIAN_POINT('',(-3.13132109303527,-3.6,8.79263101785268));
#11509=CARTESIAN_POINT('Origin',(-2.82632109303527,-2.7,8.79263101785268));
#11510=CARTESIAN_POINT('Origin',(-6.81682937671534,-3.5,16.2976855571536));
#11511=CARTESIAN_POINT('',(-6.1383908997902,-2.7,15.873750145767));
#11512=CARTESIAN_POINT('',(-6.1383908997902,-3.5,15.873750145767));
#11513=CARTESIAN_POINT('',(-6.1383908997902,-3.5,15.873750145767));
#11514=CARTESIAN_POINT('',(-6.84474897407734,-2.7,15.4981728955383));
#11515=CARTESIAN_POINT('Origin',(-6.81682937671534,-2.7,16.2976855571536));
#11516=CARTESIAN_POINT('',(-6.84474897407734,-3.5,15.4981728955383));
#11517=CARTESIAN_POINT('',(-6.84474897407734,-3.5,15.4981728955383));
#11518=CARTESIAN_POINT('Origin',(-6.81682937671534,-3.5,16.2976855571536));
#11519=CARTESIAN_POINT('Origin',(-4.,-3.5,11.));
#11520=CARTESIAN_POINT('',(-4.78345683176268,-3.5,11.6214462106767));
#11521=CARTESIAN_POINT('',(-4.35317903714357,-3.5,10.8122113748856));
#11522=CARTESIAN_POINT('',(-5.,-3.5,11.));
#11523=CARTESIAN_POINT('Origin',(-4.,-3.5,11.));
#11524=CARTESIAN_POINT('',(-3.92290124252446,-3.5,10.0029765390946));
#11525=CARTESIAN_POINT('Origin',(-4.,-3.5,11.));
#11526=CARTESIAN_POINT('',(-3.44919101049801,-3.5,9.11205716881713));
#11527=CARTESIAN_POINT('',(-3.17950013017884,-3.5,8.60484239273833));
#11528=CARTESIAN_POINT('',(-2.74283293621087,-3.5,9.48763441904585));
#11529=CARTESIAN_POINT('Origin',(-2.82632109303527,-3.5,8.79263101785268));
#11530=CARTESIAN_POINT('',(-3.21654316823732,-3.5,10.3785537893233));
#11531=CARTESIAN_POINT('',(-3.64682096285643,-3.5,11.1877886251144));
#11532=CARTESIAN_POINT('',(-4.07709875747554,-3.5,11.9970234609054));
#11533=CARTESIAN_POINT('Origin',(-4.,-3.5,11.));
#11534=CARTESIAN_POINT('',(-6.46365033957177,-3.5,16.4854741822679));
#11535=CARTESIAN_POINT('',(-4.5,-3.5,11.));
#11536=CARTESIAN_POINT('Origin',(-4.,-3.5,11.));
#11537=CARTESIAN_POINT('Origin',(-4.35317903714357,-3.5,10.8122113748856));
#11538=CARTESIAN_POINT('',(-4.78345683176268,-2.7,11.6214462106767));
#11539=CARTESIAN_POINT('',(-4.35317903714357,-2.7,10.8122113748856));
#11540=CARTESIAN_POINT('',(-4.78345683176268,-3.5,11.6214462106767));
#11541=CARTESIAN_POINT('Origin',(-5.40841468835767,-2.7,13.6488427785768));
#11542=CARTESIAN_POINT('',(-4.07709875747554,-2.7,11.9970234609054));
#11543=CARTESIAN_POINT('',(-6.46365033957177,-2.7,16.4854741822679));
#11544=CARTESIAN_POINT('Origin',(-4.,-2.7,11.));
#11545=CARTESIAN_POINT('Origin',(-6.46365033957177,-3.5,16.4854741822679));
#11546=CARTESIAN_POINT('',(-4.07709875747554,-3.5,11.9970234609054));
#11547=CARTESIAN_POINT('Origin',(-2.82632109303527,-3.5,8.79263101785268));
#11548=CARTESIAN_POINT('',(-3.44919101049801,-2.7,9.11205716881713));
#11549=CARTESIAN_POINT('',(-3.44919101049801,-3.5,9.11205716881713));
#11550=CARTESIAN_POINT('',(-2.74283293621087,-2.7,9.48763441904585));
#11551=CARTESIAN_POINT('Origin',(-2.82632109303527,-2.7,8.79263101785268));
#11552=CARTESIAN_POINT('',(-2.74283293621087,-3.5,9.48763441904585));
#11553=CARTESIAN_POINT('Origin',(-3.64682096285643,-3.5,11.1877886251144));
#11554=CARTESIAN_POINT('',(-3.21654316823732,-2.7,10.3785537893233));
#11555=CARTESIAN_POINT('',(-3.64682096285643,-2.7,11.1877886251144));
#11556=CARTESIAN_POINT('',(-3.21654316823732,-3.5,10.3785537893233));
#11557=CARTESIAN_POINT('Origin',(-3.41316054651764,-2.7,9.89631550892634));
#11558=CARTESIAN_POINT('',(-3.92290124252446,-2.7,10.0029765390946));
#11559=CARTESIAN_POINT('',(-3.17950013017884,-2.7,8.60484239273833));
#11560=CARTESIAN_POINT('Origin',(-4.,-2.7,11.));
#11561=CARTESIAN_POINT('Origin',(-3.17950013017884,-3.5,8.60484239273833));
#11562=CARTESIAN_POINT('',(-3.92290124252446,-3.5,10.0029765390946));
#11563=CARTESIAN_POINT('Origin',(-4.,-2.,11.));
#11564=CARTESIAN_POINT('',(-5.,-2.,11.));
#11565=CARTESIAN_POINT('Origin',(-4.,-2.,11.));
#11566=CARTESIAN_POINT('',(-4.7,-2.,11.));
#11567=CARTESIAN_POINT('Origin',(-4.,-2.,11.));
#11568=CARTESIAN_POINT('Origin',(-4.,-3.5,11.));
#11569=CARTESIAN_POINT('',(-5.,-3.5,11.));
#11570=CARTESIAN_POINT('Origin',(-4.,-0.45,11.));
#11571=CARTESIAN_POINT('',(-4.7,-0.45,11.));
#11572=CARTESIAN_POINT('Origin',(-4.,-0.45,11.));
#11573=CARTESIAN_POINT('',(-4.5,-0.45,11.));
#11574=CARTESIAN_POINT('Origin',(-4.,-0.45,11.));
#11575=CARTESIAN_POINT('Origin',(-4.,-2.,11.));
#11576=CARTESIAN_POINT('',(-4.7,-2.,11.));
#11577=CARTESIAN_POINT('Origin',(-4.,-4.,11.));
#11578=CARTESIAN_POINT('',(-4.5,-4.,11.));
#11579=CARTESIAN_POINT('',(-4.5,-4.,11.));
#11580=CARTESIAN_POINT('Origin',(-4.,-4.,11.));
#11581=CARTESIAN_POINT('Origin',(-4.,-4.,11.));
#11582=CARTESIAN_POINT('',(-4.5,1.8,11.));
#11583=CARTESIAN_POINT('Origin',(-4.,1.8,11.));
#11584=CARTESIAN_POINT('',(-4.5,-4.,11.));
#11585=CARTESIAN_POINT('Origin',(-4.,1.8,11.));
#11586=CARTESIAN_POINT('Origin',(-4.,-4.,11.));
#11587=CARTESIAN_POINT('',(0.,0.,0.));
#11588=CARTESIAN_POINT('Origin',(-4.,0.45,11.));
#11589=CARTESIAN_POINT('',(-4.505,1.,11.));
#11590=CARTESIAN_POINT('Origin',(-4.,1.,11.));
#11591=CARTESIAN_POINT('',(-4.505,0.45,11.));
#11592=CARTESIAN_POINT('',(-4.505,0.45,11.));
#11593=CARTESIAN_POINT('Origin',(-4.,0.45,11.));
#11594=CARTESIAN_POINT('Origin',(-4.,0.45,11.));
#11595=CARTESIAN_POINT('',(-4.7,1.,11.));
#11596=CARTESIAN_POINT('Origin',(-4.,1.,11.));
#11597=CARTESIAN_POINT('',(-4.7,0.45,11.));
#11598=CARTESIAN_POINT('',(-4.7,0.45,11.));
#11599=CARTESIAN_POINT('Origin',(-4.,0.45,11.));
#11600=CARTESIAN_POINT('Origin',(-4.,1.,11.));
#11601=CARTESIAN_POINT('Origin',(-4.,0.45,11.));
#11602=CARTESIAN_POINT('',(0.,0.,0.));
#11603=CARTESIAN_POINT('Origin',(-3.51,1.4,11.));
#11604=CARTESIAN_POINT('',(-3.51,1.28909463493591,10.8778320827713));
#11605=CARTESIAN_POINT('',(-3.51,1.51090536506409,10.8778320827713));
#11606=CARTESIAN_POINT('',(-3.51,1.,10.8778320827713));
#11607=CARTESIAN_POINT('Origin',(-3.51,1.4,11.));
#11608=CARTESIAN_POINT('Origin',(-3.51,1.4,11.));
#11609=CARTESIAN_POINT('',(-3.51,1.28909463493591,11.1221679172287));
#11610=CARTESIAN_POINT('Ctrl Pts',(-3.51,1.28909463493591,11.1221679172287));
#11611=CARTESIAN_POINT('Ctrl Pts',(-3.50955146832001,1.28711294069536,11.1203689136263));
#11612=CARTESIAN_POINT('Ctrl Pts',(-3.50910475462832,1.28518965877367,11.1185348965652));
#11613=CARTESIAN_POINT('Ctrl Pts',(-3.50520498446835,1.2687667552278,11.1021119930194));
#11614=CARTESIAN_POINT('Ctrl Pts',(-3.50155748539241,1.25609154388858,11.0836597150224));
#11615=CARTESIAN_POINT('Ctrl Pts',(-3.49642218023894,1.23920409039234,11.0430495960472));
#11616=CARTESIAN_POINT('Ctrl Pts',(-3.495,1.235,11.0208800943307));
#11617=CARTESIAN_POINT('Ctrl Pts',(-3.495,1.235,10.9791199056693));
#11618=CARTESIAN_POINT('Ctrl Pts',(-3.49642218023894,1.23920409039234,10.9569504039528));
#11619=CARTESIAN_POINT('Ctrl Pts',(-3.50155748539241,1.25609154388858,10.9163402849776));
#11620=CARTESIAN_POINT('Ctrl Pts',(-3.50520498446835,1.2687667552278,10.8978880069806));
#11621=CARTESIAN_POINT('Ctrl Pts',(-3.50910475462832,1.28518965877367,10.8814651034348));
#11622=CARTESIAN_POINT('Ctrl Pts',(-3.50955146832001,1.28711294069536,10.8796310863737));
#11623=CARTESIAN_POINT('Ctrl Pts',(-3.51,1.28909463493591,10.8778320827713));
#11624=CARTESIAN_POINT('',(-3.51,1.4,11.165));
#11625=CARTESIAN_POINT('Origin',(-3.51,1.4,11.));
#11626=CARTESIAN_POINT('',(-3.11525427381648,1.4,11.165));
#11627=CARTESIAN_POINT('',(-3.51,1.4,11.165));
#11628=CARTESIAN_POINT('',(-3.11525427381648,1.4,10.835));
#11629=CARTESIAN_POINT('Ctrl Pts',(-3.11525427381648,1.4,10.835));
#11630=CARTESIAN_POINT('Ctrl Pts',(-3.11525427381648,1.37923124059256,10.835));
#11631=CARTESIAN_POINT('Ctrl Pts',(-3.11444724049474,1.35711110492666,10.8391602809924));
#11632=CARTESIAN_POINT('Ctrl Pts',(-3.11155135184996,1.31647293736623,10.8560135297833));
#11633=CARTESIAN_POINT('Ctrl Pts',(-3.10950639514836,1.29795075602263,10.8687040061858));
#11634=CARTESIAN_POINT('Ctrl Pts',(-3.10568276567606,1.26870458121656,10.8979501809919));
#11635=CARTESIAN_POINT('Ctrl Pts',(-3.10365291110046,1.25601365401642,10.9164726079093));
#11636=CARTESIAN_POINT('Ctrl Pts',(-3.10079172813942,1.23916007816136,10.9571116239066));
#11637=CARTESIAN_POINT('Ctrl Pts',(-3.1,1.235,10.9792320572765));
#11638=CARTESIAN_POINT('Ctrl Pts',(-3.1,1.235,11.0207679427235));
#11639=CARTESIAN_POINT('Ctrl Pts',(-3.10079172813942,1.23916007816136,11.0428883760934));
#11640=CARTESIAN_POINT('Ctrl Pts',(-3.10365291110046,1.25601365401642,11.0835273920907));
#11641=CARTESIAN_POINT('Ctrl Pts',(-3.10568276567606,1.26870458121656,11.1020498190081));
#11642=CARTESIAN_POINT('Ctrl Pts',(-3.10950639514836,1.29795075602263,11.1312959938142));
#11643=CARTESIAN_POINT('Ctrl Pts',(-3.11155135184996,1.31647293736623,11.1439864702167));
#11644=CARTESIAN_POINT('Ctrl Pts',(-3.11444724049474,1.35711110492666,11.1608397190076));
#11645=CARTESIAN_POINT('Ctrl Pts',(-3.11525427381648,1.37923124059256,11.165));
#11646=CARTESIAN_POINT('Ctrl Pts',(-3.11525427381648,1.4,11.165));
#11647=CARTESIAN_POINT('Ctrl Pts',(-3.11525427381648,1.4,11.165));
#11648=CARTESIAN_POINT('Ctrl Pts',(-3.11525427381648,1.42076875940744,11.165));
#11649=CARTESIAN_POINT('Ctrl Pts',(-3.11444724049474,1.44288889507334,11.1608397190076));
#11650=CARTESIAN_POINT('Ctrl Pts',(-3.11155135184996,1.48352706263377,11.1439864702167));
#11651=CARTESIAN_POINT('Ctrl Pts',(-3.10950639514836,1.50204924397737,11.1312959938142));
#11652=CARTESIAN_POINT('Ctrl Pts',(-3.10568276567606,1.53129541878343,11.1020498190081));
#11653=CARTESIAN_POINT('Ctrl Pts',(-3.10365291110046,1.54398634598358,11.0835273920907));
#11654=CARTESIAN_POINT('Ctrl Pts',(-3.10079172813942,1.56083992183864,11.0428883760934));
#11655=CARTESIAN_POINT('Ctrl Pts',(-3.1,1.565,11.0207679427235));
#11656=CARTESIAN_POINT('Ctrl Pts',(-3.1,1.565,10.9792320572765));
#11657=CARTESIAN_POINT('Ctrl Pts',(-3.10079172813942,1.56083992183864,10.9571116239066));
#11658=CARTESIAN_POINT('Ctrl Pts',(-3.10365291110046,1.54398634598358,10.9164726079093));
#11659=CARTESIAN_POINT('Ctrl Pts',(-3.10568276567606,1.53129541878343,10.8979501809919));
#11660=CARTESIAN_POINT('Ctrl Pts',(-3.10950639514836,1.50204924397737,10.8687040061858));
#11661=CARTESIAN_POINT('Ctrl Pts',(-3.11155135184996,1.48352706263377,10.8560135297833));
#11662=CARTESIAN_POINT('Ctrl Pts',(-3.11444724049474,1.44288889507334,10.8391602809924));
#11663=CARTESIAN_POINT('Ctrl Pts',(-3.11525427381648,1.42076875940744,10.835));
#11664=CARTESIAN_POINT('Ctrl Pts',(-3.11525427381648,1.4,10.835));
#11665=CARTESIAN_POINT('',(-3.51,1.51090536506409,11.1221679172287));
#11666=CARTESIAN_POINT('Origin',(-3.51,1.4,11.));
#11667=CARTESIAN_POINT('Ctrl Pts',(-3.51,1.51090536506409,10.8778320827713));
#11668=CARTESIAN_POINT('Ctrl Pts',(-3.50955146832001,1.51288705930464,10.8796310863737));
#11669=CARTESIAN_POINT('Ctrl Pts',(-3.50910475462832,1.51481034122633,10.8814651034348));
#11670=CARTESIAN_POINT('Ctrl Pts',(-3.50520498446835,1.5312332447722,10.8978880069806));
#11671=CARTESIAN_POINT('Ctrl Pts',(-3.50155748539241,1.54390845611142,10.9163402849776));
#11672=CARTESIAN_POINT('Ctrl Pts',(-3.49642218023894,1.56079590960766,10.9569504039528));
#11673=CARTESIAN_POINT('Ctrl Pts',(-3.495,1.565,10.9791199056693));
#11674=CARTESIAN_POINT('Ctrl Pts',(-3.495,1.565,11.0208800943307));
#11675=CARTESIAN_POINT('Ctrl Pts',(-3.49642218023894,1.56079590960766,11.0430495960472));
#11676=CARTESIAN_POINT('Ctrl Pts',(-3.50155748539241,1.54390845611142,11.0836597150224));
#11677=CARTESIAN_POINT('Ctrl Pts',(-3.50520498446835,1.5312332447722,11.1021119930194));
#11678=CARTESIAN_POINT('Ctrl Pts',(-3.50910475462832,1.51481034122633,11.1185348965652));
#11679=CARTESIAN_POINT('Ctrl Pts',(-3.50955146832001,1.51288705930464,11.1203689136263));
#11680=CARTESIAN_POINT('Ctrl Pts',(-3.51,1.51090536506409,11.1221679172287));
#11681=CARTESIAN_POINT('Origin',(-3.51,1.4,11.));
#11682=CARTESIAN_POINT('',(-3.51,1.,11.1221679172287));
#11683=CARTESIAN_POINT('Origin',(-4.,1.,11.));
#11684=CARTESIAN_POINT('',(-4.505,1.8,11.));
#11685=CARTESIAN_POINT('Origin',(-4.,1.8,11.));
#11686=CARTESIAN_POINT('',(-4.505,1.,11.));
#11687=CARTESIAN_POINT('',(-4.505,1.,11.));
#11688=CARTESIAN_POINT('Origin',(-4.,1.,11.));
#11689=CARTESIAN_POINT('Origin',(-4.,1.,11.));
#11690=CARTESIAN_POINT('',(-4.9,1.8,11.));
#11691=CARTESIAN_POINT('Origin',(-4.,1.8,11.));
#11692=CARTESIAN_POINT('',(-4.9,1.,11.));
#11693=CARTESIAN_POINT('',(-4.9,1.,11.));
#11694=CARTESIAN_POINT('Origin',(-4.,1.,11.));
#11695=CARTESIAN_POINT('Origin',(-4.,1.8,11.));
#11696=CARTESIAN_POINT('Origin',(-4.,1.,11.));
#11697=CARTESIAN_POINT('',(0.,0.,0.));
#11698=CARTESIAN_POINT('Origin',(-2.82632109303527,-4.2,8.79263101785268));
#11699=CARTESIAN_POINT('',(-2.99132109303527,-4.2,8.79263101785268));
#11700=CARTESIAN_POINT('Origin',(-2.82632109303527,-4.2,8.79263101785268));
#11701=CARTESIAN_POINT('',(-2.99132109303527,-2.7,8.79263101785268));
#11702=CARTESIAN_POINT('',(-2.99132109303527,-4.2,8.79263101785268));
#11703=CARTESIAN_POINT('Origin',(-2.82632109303527,-2.7,8.79263101785268));
#11704=CARTESIAN_POINT('Origin',(-2.82632109303527,-4.2,8.79263101785268));
#11705=CARTESIAN_POINT('Origin',(-2.82632109303527,-5.8,8.79263101785268));
#11706=CARTESIAN_POINT('',(-2.99132109303527,-5.7,8.79263101785268));
#11707=CARTESIAN_POINT('Origin',(-2.82632109303527,-5.7,8.79263101785268));
#11708=CARTESIAN_POINT('',(-2.99132109303527,-4.7,8.79263101785268));
#11709=CARTESIAN_POINT('',(-2.99132109303527,-5.8,8.79263101785268));
#11710=CARTESIAN_POINT('Origin',(-2.82632109303527,-4.7,8.79263101785268));
#11711=CARTESIAN_POINT('Origin',(-2.82632109303527,-4.7,8.79263101785268));
#11712=CARTESIAN_POINT('Origin',(-2.82632109303527,-3.5,8.79263101785268));
#11713=CARTESIAN_POINT('',(-3.52632109303527,-3.5,8.79263101785268));
#11714=CARTESIAN_POINT('Origin',(-2.82632109303527,-3.5,8.79263101785268));
#11715=CARTESIAN_POINT('',(-3.12632109303527,-3.5,8.79263101785268));
#11716=CARTESIAN_POINT('Origin',(-2.82632109303527,-3.5,8.79263101785268));
#11717=CARTESIAN_POINT('Origin',(-2.82632109303527,-3.9,8.79263101785268));
#11718=CARTESIAN_POINT('',(-3.52632109303527,-3.9,8.79263101785268));
#11719=CARTESIAN_POINT('Origin',(-2.82632109303527,-3.9,8.79263101785268));
#11720=CARTESIAN_POINT('',(-3.12632109303527,-3.9,8.79263101785268));
#11721=CARTESIAN_POINT('Origin',(-2.82632109303527,-3.9,8.79263101785268));
#11722=CARTESIAN_POINT('Origin',(-2.82632109303527,-3.9,8.79263101785268));
#11723=CARTESIAN_POINT('',(-3.52632109303527,-3.9,8.79263101785268));
#11724=CARTESIAN_POINT('Origin',(-2.82632109303527,-5.7,8.79263101785268));
#11725=CARTESIAN_POINT('',(-3.12632109303527,-5.7,8.79263101785268));
#11726=CARTESIAN_POINT('',(-3.12632109303527,-5.7,8.79263101785268));
#11727=CARTESIAN_POINT('Origin',(-2.82632109303527,-5.7,8.79263101785268));
#11728=CARTESIAN_POINT('Origin',(-2.82632109303527,-5.7,8.79263101785268));
#11729=CARTESIAN_POINT('',(-3.12632109303527,-2.7,8.79263101785268));
#11730=CARTESIAN_POINT('Origin',(-2.82632109303527,-2.7,8.79263101785268));
#11731=CARTESIAN_POINT('',(-3.12632109303527,-5.7,8.79263101785268));
#11732=CARTESIAN_POINT('Origin',(-2.82632109303527,-2.7,8.79263101785268));
#11733=CARTESIAN_POINT('Origin',(-2.82632109303527,-5.7,8.79263101785268));
#11734=CARTESIAN_POINT('',(0.,0.,0.));
#11735=CARTESIAN_POINT('Origin',(-2.82632109303527,-4.7,8.79263101785268));
#11736=CARTESIAN_POINT('',(-3.13132109303527,-3.9,8.79263101785268));
#11737=CARTESIAN_POINT('Origin',(-2.82632109303527,-3.9,8.79263101785268));
#11738=CARTESIAN_POINT('',(-3.13132109303527,-4.7,8.79263101785268));
#11739=CARTESIAN_POINT('',(-3.13132109303527,-4.7,8.79263101785268));
#11740=CARTESIAN_POINT('Origin',(-2.82632109303527,-4.7,8.79263101785268));
#11741=CARTESIAN_POINT('Origin',(-2.82632109303527,-4.7,8.79263101785268));
#11742=CARTESIAN_POINT('',(-3.32632109303527,-3.9,8.79263101785268));
#11743=CARTESIAN_POINT('Origin',(-2.82632109303527,-3.9,8.79263101785268));
#11744=CARTESIAN_POINT('',(-3.32632109303527,-4.7,8.79263101785268));
#11745=CARTESIAN_POINT('',(-3.32632109303527,-4.7,8.79263101785268));
#11746=CARTESIAN_POINT('Origin',(-2.82632109303527,-4.7,8.79263101785268));
#11747=CARTESIAN_POINT('Origin',(-2.82632109303527,-3.9,8.79263101785268));
#11748=CARTESIAN_POINT('Origin',(-2.82632109303527,-4.7,8.79263101785268));
#11749=CARTESIAN_POINT('',(0.,0.,0.));
#11750=CARTESIAN_POINT('Origin',(-2.82632109303527,-5.7,8.79263101785268));
#11751=CARTESIAN_POINT('',(-3.13132109303527,-5.5,8.79263101785268));
#11752=CARTESIAN_POINT('Origin',(-2.82632109303527,-5.5,8.79263101785268));
#11753=CARTESIAN_POINT('',(-3.13132109303527,-5.7,8.79263101785268));
#11754=CARTESIAN_POINT('',(-3.13132109303527,-5.7,8.79263101785268));
#11755=CARTESIAN_POINT('Origin',(-2.82632109303527,-5.7,8.79263101785268));
#11756=CARTESIAN_POINT('Origin',(-2.82632109303527,-5.7,8.79263101785268));
#11757=CARTESIAN_POINT('',(-3.32632109303527,-5.5,8.79263101785268));
#11758=CARTESIAN_POINT('Origin',(-2.82632109303527,-5.5,8.79263101785268));
#11759=CARTESIAN_POINT('',(-3.32632109303527,-5.7,8.79263101785268));
#11760=CARTESIAN_POINT('',(-3.32632109303527,-5.7,8.79263101785268));
#11761=CARTESIAN_POINT('Origin',(-2.82632109303527,-5.7,8.79263101785268));
#11762=CARTESIAN_POINT('Origin',(-2.82632109303527,-5.5,8.79263101785268));
#11763=CARTESIAN_POINT('Origin',(-2.82632109303527,-5.7,8.79263101785268));
#11764=CARTESIAN_POINT('',(0.,0.,0.));
#11765=CARTESIAN_POINT('Origin',(-2.82632109303527,-5.9,8.79263101785268));
#11766=CARTESIAN_POINT('',(-3.05132109303527,-5.7,8.79263101785268));
#11767=CARTESIAN_POINT('Origin',(-2.82632109303527,-5.7,8.79263101785268));
#11768=CARTESIAN_POINT('',(-3.05132109303527,-5.9,8.79263101785268));
#11769=CARTESIAN_POINT('',(-3.05132109303527,-5.9,8.79263101785268));
#11770=CARTESIAN_POINT('Origin',(-2.82632109303527,-5.9,8.79263101785268));
#11771=CARTESIAN_POINT('Origin',(-2.82632109303527,-5.9,8.79263101785268));
#11772=CARTESIAN_POINT('',(-3.32632109303527,-5.7,8.79263101785268));
#11773=CARTESIAN_POINT('Origin',(-2.82632109303527,-5.7,8.79263101785268));
#11774=CARTESIAN_POINT('',(-3.32632109303527,-5.9,8.79263101785268));
#11775=CARTESIAN_POINT('',(-3.32632109303527,-5.9,8.79263101785268));
#11776=CARTESIAN_POINT('Origin',(-2.82632109303527,-5.9,8.79263101785268));
#11777=CARTESIAN_POINT('Origin',(-2.82632109303527,-5.7,8.79263101785268));
#11778=CARTESIAN_POINT('Origin',(-2.82632109303527,-5.9,8.79263101785268));
#11779=CARTESIAN_POINT('',(0.,0.,0.));
#11780=CARTESIAN_POINT('Origin',(-2.82632109303527,-2.7,8.79263101785268));
#11781=CARTESIAN_POINT('',(-3.05132109303527,-2.5,8.79263101785268));
#11782=CARTESIAN_POINT('Origin',(-2.82632109303527,-2.5,8.79263101785268));
#11783=CARTESIAN_POINT('',(-3.05132109303527,-2.7,8.79263101785268));
#11784=CARTESIAN_POINT('',(-3.05132109303527,-2.7,8.79263101785268));
#11785=CARTESIAN_POINT('Origin',(-2.82632109303527,-2.7,8.79263101785268));
#11786=CARTESIAN_POINT('Origin',(-2.82632109303527,-2.7,8.79263101785268));
#11787=CARTESIAN_POINT('',(-3.32632109303527,-2.5,8.79263101785268));
#11788=CARTESIAN_POINT('Origin',(-2.82632109303527,-2.5,8.79263101785268));
#11789=CARTESIAN_POINT('',(-3.32632109303527,-2.7,8.79263101785268));
#11790=CARTESIAN_POINT('',(-3.32632109303527,-2.7,8.79263101785268));
#11791=CARTESIAN_POINT('Origin',(-2.82632109303527,-2.7,8.79263101785268));
#11792=CARTESIAN_POINT('Origin',(-2.82632109303527,-2.5,8.79263101785268));
#11793=CARTESIAN_POINT('Origin',(-2.82632109303527,-2.7,8.79263101785268));
#11794=CARTESIAN_POINT('',(0.,0.,0.));
#11795=CARTESIAN_POINT('Origin',(0.,-0.4,0.));
#11796=CARTESIAN_POINT('',(-0.1954,-0.4,2.39295984553393E-17));
#11797=CARTESIAN_POINT('Origin',(0.,-0.4,0.));
#11798=CARTESIAN_POINT('Origin',(0.0577350269189626,0.,-0.1));
#11799=CARTESIAN_POINT('',(0.0577350269189626,0.,-0.1));
#11800=CARTESIAN_POINT('',(0.115470053837925,0.,0.));
#11801=CARTESIAN_POINT('',(0.0934187836487032,0.,-0.0381939203391614));
#11802=CARTESIAN_POINT('',(0.0577350269189626,-0.2,-0.1));
#11803=CARTESIAN_POINT('',(0.0577350269189626,0.,-0.1));
#11804=CARTESIAN_POINT('',(0.115470053837925,-0.2,0.));
#11805=CARTESIAN_POINT('',(0.115470053837925,-0.2,0.));
#11806=CARTESIAN_POINT('',(0.115470053837925,0.,0.));
#11807=CARTESIAN_POINT('Origin',(-0.0577350269189626,0.,-0.1));
#11808=CARTESIAN_POINT('',(-0.0577350269189626,0.,-0.1));
#11809=CARTESIAN_POINT('',(0.0561324865405187,0.,-0.1));
#11810=CARTESIAN_POINT('',(-0.0577350269189626,-0.2,-0.1));
#11811=CARTESIAN_POINT('',(-0.0577350269189626,0.,-0.1));
#11812=CARTESIAN_POINT('',(0.0577350269189626,-0.2,-0.1));
#11813=CARTESIAN_POINT('Origin',(-0.115470053837925,0.,-1.38777878078145E-17));
#11814=CARTESIAN_POINT('',(-0.115470053837925,0.,-1.41410031829988E-17));
#11815=CARTESIAN_POINT('',(-0.0797862971081845,0.,-0.0618060796608387));
#11816=CARTESIAN_POINT('',(-0.115470053837925,-0.2,-1.38777878078145E-17));
#11817=CARTESIAN_POINT('',(-0.115470053837925,0.,-1.41410031829988E-17));
#11818=CARTESIAN_POINT('',(-0.0577350269189626,-0.2,-0.1));
#11819=CARTESIAN_POINT('Origin',(-0.0577350269189626,0.,0.1));
#11820=CARTESIAN_POINT('',(-0.0577350269189626,0.,0.1));
#11821=CARTESIAN_POINT('',(-0.0509187836487033,0.,0.111806079660839));
#11822=CARTESIAN_POINT('',(-0.0577350269189626,-0.2,0.1));
#11823=CARTESIAN_POINT('',(-0.0577350269189626,0.,0.1));
#11824=CARTESIAN_POINT('',(-0.115470053837925,-0.2,-1.41410031829988E-17));
#11825=CARTESIAN_POINT('Origin',(0.0577350269189626,0.,0.1));
#11826=CARTESIAN_POINT('',(0.0577350269189626,0.,0.1));
#11827=CARTESIAN_POINT('',(0.113867513459481,0.,0.1));
#11828=CARTESIAN_POINT('',(0.0577350269189626,-0.2,0.1));
#11829=CARTESIAN_POINT('',(0.0577350269189626,0.,0.1));
#11830=CARTESIAN_POINT('',(-0.0577350269189626,-0.2,0.1));
#11831=CARTESIAN_POINT('Origin',(0.115470053837925,0.,0.));
#11832=CARTESIAN_POINT('',(0.122286297108185,0.,-0.0118060796608386));
#11833=CARTESIAN_POINT('',(0.0577350269189626,-0.2,0.1));
#11834=CARTESIAN_POINT('Origin',(0.,-0.2,0.));
#11835=CARTESIAN_POINT('Origin',(0.17,0.,0.));
#11836=CARTESIAN_POINT('',(-0.17,-8.67361737988404E-18,-2.0818995585505E-17));
#11837=CARTESIAN_POINT('Origin',(0.,0.,0.));
#11838=CARTESIAN_POINT('Origin',(0.,-0.015,0.));
#11839=CARTESIAN_POINT('',(-0.1954,-0.0254,-2.39295984553393E-17));
#11840=CARTESIAN_POINT('Origin',(0.,-0.0254,0.));
#11841=CARTESIAN_POINT('',(-0.185,-0.015,-2.2655965784226E-17));
#11842=CARTESIAN_POINT('Origin',(0.,-0.2775,0.));
#11843=CARTESIAN_POINT('',(-0.1954,-0.2775,-2.39295984553393E-17));
#11844=CARTESIAN_POINT('',(0.,0.,0.));
#11845=CARTESIAN_POINT('Origin',(0.0866025403784439,-0.4,-0.15));
#11846=CARTESIAN_POINT('',(0.173205080756888,-0.4,0.));
#11847=CARTESIAN_POINT('',(0.0866025403784439,-0.4,-0.15));
#11848=CARTESIAN_POINT('',(0.173205080756888,-0.4,0.));
#11849=CARTESIAN_POINT('',(0.0866025403784439,-0.64,-0.15));
#11850=CARTESIAN_POINT('',(0.0866025403784439,-0.4,-0.15));
#11851=CARTESIAN_POINT('',(0.173205080756888,-0.64,0.));
#11852=CARTESIAN_POINT('',(0.173205080756888,-0.64,0.));
#11853=CARTESIAN_POINT('',(0.173205080756888,-0.4,0.));
#11854=CARTESIAN_POINT('Origin',(-0.0866025403784438,-0.4,-0.15));
#11855=CARTESIAN_POINT('',(-0.0866025403784438,-0.4,-0.15));
#11856=CARTESIAN_POINT('',(0.0866025403784439,-0.4,-0.15));
#11857=CARTESIAN_POINT('',(-0.0866025403784438,-0.64,-0.15));
#11858=CARTESIAN_POINT('',(-0.0866025403784438,-0.4,-0.15));
#11859=CARTESIAN_POINT('',(0.0866025403784439,-0.64,-0.15));
#11860=CARTESIAN_POINT('Origin',(-0.173205080756888,-0.4,-2.77555756156289E-17));
#11861=CARTESIAN_POINT('',(-0.173205080756888,-0.4,-2.12115047744981E-17));
#11862=CARTESIAN_POINT('',(-0.0866025403784438,-0.4,-0.15));
#11863=CARTESIAN_POINT('',(-0.173205080756888,-0.64,-2.77555756156289E-17));
#11864=CARTESIAN_POINT('',(-0.173205080756888,-0.4,-2.12115047744981E-17));
#11865=CARTESIAN_POINT('',(-0.0866025403784438,-0.64,-0.15));
#11866=CARTESIAN_POINT('Origin',(-0.0866025403784439,-0.4,0.15));
#11867=CARTESIAN_POINT('',(-0.0866025403784439,-0.4,0.15));
#11868=CARTESIAN_POINT('',(-0.173205080756888,-0.4,-2.12115047744981E-17));
#11869=CARTESIAN_POINT('',(-0.0866025403784439,-0.64,0.15));
#11870=CARTESIAN_POINT('',(-0.0866025403784439,-0.4,0.15));
#11871=CARTESIAN_POINT('',(-0.173205080756888,-0.64,-2.12115047744981E-17));
#11872=CARTESIAN_POINT('Origin',(0.0866025403784439,-0.4,0.15));
#11873=CARTESIAN_POINT('',(0.0866025403784439,-0.4,0.15));
#11874=CARTESIAN_POINT('',(-0.0866025403784439,-0.4,0.15));
#11875=CARTESIAN_POINT('',(0.0866025403784439,-0.64,0.15));
#11876=CARTESIAN_POINT('',(0.0866025403784439,-0.4,0.15));
#11877=CARTESIAN_POINT('',(-0.0866025403784439,-0.64,0.15));
#11878=CARTESIAN_POINT('Origin',(0.173205080756888,-0.4,0.));
#11879=CARTESIAN_POINT('',(0.0866025403784439,-0.4,0.15));
#11880=CARTESIAN_POINT('',(0.0866025403784439,-0.64,0.15));
#11881=CARTESIAN_POINT('Origin',(0.,-0.4,-2.77555756156289E-17));
#11882=CARTESIAN_POINT('Origin',(0.,-0.64,-2.77555756156289E-17));
#11883=CARTESIAN_POINT('Origin',(0.,-1.,0.));
#11884=CARTESIAN_POINT('',(-0.1954,-1.,2.39295984553393E-17));
#11885=CARTESIAN_POINT('Origin',(0.,-1.,0.));
#11886=CARTESIAN_POINT('Origin',(0.3,0.4,0.));
#11887=CARTESIAN_POINT('',(-0.3,0.4,-3.67394039744206E-17));
#11888=CARTESIAN_POINT('Origin',(0.,0.4,0.));
#11889=CARTESIAN_POINT('Origin',(0.,0.375,0.));
#11890=CARTESIAN_POINT('',(-0.35,0.35,-4.28626379701573E-17));
#11891=CARTESIAN_POINT('Origin',(0.,0.35,0.));
#11892=CARTESIAN_POINT('',(-0.325,0.375,-3.9801020972289E-17));
#11893=CARTESIAN_POINT('Origin',(0.,0.19,0.));
#11894=CARTESIAN_POINT('',(-0.35,0.03,-4.28626379701574E-17));
#11895=CARTESIAN_POINT('Origin',(0.,0.03,0.));
#11896=CARTESIAN_POINT('',(-0.35,0.19,-4.28626379701574E-17));
#11897=CARTESIAN_POINT('Origin',(0.,0.0149999999999999,0.));
#11898=CARTESIAN_POINT('',(-0.32,-3.29597460435593E-17,-3.91886975727153E-17));
#11899=CARTESIAN_POINT('Origin',(0.,0.,0.));
#11900=CARTESIAN_POINT('',(-0.335,0.0149999999999999,-4.10256677714363E-17));
#11901=CARTESIAN_POINT('Origin',(0.22,0.,0.));
#11902=CARTESIAN_POINT('',(-0.22,-6.93889390390723E-18,-2.69422295812418E-17));
#11903=CARTESIAN_POINT('Origin',(0.,0.,0.));
#11904=CARTESIAN_POINT('Origin',(0.,-0.02,0.));
#11905=CARTESIAN_POINT('',(-0.1954,-0.0492,2.39295984553393E-17));
#11906=CARTESIAN_POINT('Origin',(0.,-0.0492,0.));
#11907=CARTESIAN_POINT('',(-0.21,-0.02,-2.57175827820944E-17));
#11908=CARTESIAN_POINT('Origin',(0.,-0.8,0.));
#11909=CARTESIAN_POINT('',(-0.1954,-0.8,-2.39295984553393E-17));
#11910=CARTESIAN_POINT('',(0.,0.,0.));
#11911=CARTESIAN_POINT('Origin',(0.3,0.4,0.));
#11912=CARTESIAN_POINT('',(-0.3,0.4,-3.67394039744206E-17));
#11913=CARTESIAN_POINT('Origin',(0.,0.4,0.));
#11914=CARTESIAN_POINT('Origin',(0.,0.375,0.));
#11915=CARTESIAN_POINT('',(-0.35,0.35,-4.28626379701573E-17));
#11916=CARTESIAN_POINT('Origin',(0.,0.35,0.));
#11917=CARTESIAN_POINT('',(-0.325,0.375,-3.9801020972289E-17));
#11918=CARTESIAN_POINT('Origin',(0.,0.19,0.));
#11919=CARTESIAN_POINT('',(-0.35,0.03,-4.28626379701574E-17));
#11920=CARTESIAN_POINT('Origin',(0.,0.03,0.));
#11921=CARTESIAN_POINT('',(-0.35,0.19,-4.28626379701574E-17));
#11922=CARTESIAN_POINT('Origin',(0.,0.0149999999999999,0.));
#11923=CARTESIAN_POINT('',(-0.32,-3.29597460435593E-17,-3.91886975727153E-17));
#11924=CARTESIAN_POINT('Origin',(0.,0.,0.));
#11925=CARTESIAN_POINT('',(-0.335,0.0149999999999999,-4.10256677714363E-17));
#11926=CARTESIAN_POINT('Origin',(0.22,0.,0.));
#11927=CARTESIAN_POINT('',(-0.22,-6.93889390390723E-18,-2.69422295812418E-17));
#11928=CARTESIAN_POINT('Origin',(0.,0.,0.));
#11929=CARTESIAN_POINT('Origin',(0.,-0.02,0.));
#11930=CARTESIAN_POINT('',(-0.1954,-0.0492,2.39295984553393E-17));
#11931=CARTESIAN_POINT('Origin',(0.,-0.0492,0.));
#11932=CARTESIAN_POINT('',(-0.21,-0.02,-2.57175827820944E-17));
#11933=CARTESIAN_POINT('Origin',(0.,-0.8,0.));
#11934=CARTESIAN_POINT('',(-0.1954,-1.5646,2.39295984553393E-17));
#11935=CARTESIAN_POINT('Origin',(0.,-1.5646,0.));
#11936=CARTESIAN_POINT('',(-0.1954,-0.8,-2.39295984553393E-17));
#11937=CARTESIAN_POINT('Origin',(0.,-1.58,0.));
#11938=CARTESIAN_POINT('',(-0.16,-1.6,-1.95943487863577E-17));
#11939=CARTESIAN_POINT('Origin',(0.,-1.6,0.));
#11940=CARTESIAN_POINT('',(-0.18,-1.58,-2.20436423846524E-17));
#11941=CARTESIAN_POINT('Origin',(0.,-1.6,0.));
#11942=CARTESIAN_POINT('Origin',(0.0866025403784439,-0.4,-0.15));
#11943=CARTESIAN_POINT('',(0.173205080756888,-0.4,0.));
#11944=CARTESIAN_POINT('',(0.0866025403784439,-0.4,-0.15));
#11945=CARTESIAN_POINT('',(0.173205080756888,-0.4,0.));
#11946=CARTESIAN_POINT('',(0.0866025403784439,-0.64,-0.15));
#11947=CARTESIAN_POINT('',(0.0866025403784439,-0.4,-0.15));
#11948=CARTESIAN_POINT('',(0.173205080756888,-0.64,0.));
#11949=CARTESIAN_POINT('',(0.173205080756888,-0.64,0.));
#11950=CARTESIAN_POINT('',(0.173205080756888,-0.4,0.));
#11951=CARTESIAN_POINT('Origin',(-0.0866025403784438,-0.4,-0.15));
#11952=CARTESIAN_POINT('',(-0.0866025403784438,-0.4,-0.15));
#11953=CARTESIAN_POINT('',(0.0866025403784439,-0.4,-0.15));
#11954=CARTESIAN_POINT('',(-0.0866025403784438,-0.64,-0.15));
#11955=CARTESIAN_POINT('',(-0.0866025403784438,-0.4,-0.15));
#11956=CARTESIAN_POINT('',(0.0866025403784439,-0.64,-0.15));
#11957=CARTESIAN_POINT('Origin',(-0.173205080756888,-0.4,-2.77555756156289E-17));
#11958=CARTESIAN_POINT('',(-0.173205080756888,-0.4,-2.12115047744981E-17));
#11959=CARTESIAN_POINT('',(-0.0866025403784438,-0.4,-0.15));
#11960=CARTESIAN_POINT('',(-0.173205080756888,-0.64,-2.77555756156289E-17));
#11961=CARTESIAN_POINT('',(-0.173205080756888,-0.4,-2.12115047744981E-17));
#11962=CARTESIAN_POINT('',(-0.0866025403784438,-0.64,-0.15));
#11963=CARTESIAN_POINT('Origin',(-0.0866025403784439,-0.4,0.15));
#11964=CARTESIAN_POINT('',(-0.0866025403784439,-0.4,0.15));
#11965=CARTESIAN_POINT('',(-0.173205080756888,-0.4,-2.12115047744981E-17));
#11966=CARTESIAN_POINT('',(-0.0866025403784439,-0.64,0.15));
#11967=CARTESIAN_POINT('',(-0.0866025403784439,-0.4,0.15));
#11968=CARTESIAN_POINT('',(-0.173205080756888,-0.64,-2.12115047744981E-17));
#11969=CARTESIAN_POINT('Origin',(0.0866025403784439,-0.4,0.15));
#11970=CARTESIAN_POINT('',(0.0866025403784439,-0.4,0.15));
#11971=CARTESIAN_POINT('',(-0.0866025403784439,-0.4,0.15));
#11972=CARTESIAN_POINT('',(0.0866025403784439,-0.64,0.15));
#11973=CARTESIAN_POINT('',(0.0866025403784439,-0.4,0.15));
#11974=CARTESIAN_POINT('',(-0.0866025403784439,-0.64,0.15));
#11975=CARTESIAN_POINT('Origin',(0.173205080756888,-0.4,0.));
#11976=CARTESIAN_POINT('',(0.0866025403784439,-0.4,0.15));
#11977=CARTESIAN_POINT('',(0.0866025403784439,-0.64,0.15));
#11978=CARTESIAN_POINT('Origin',(0.,-0.4,-2.77555756156289E-17));
#11979=CARTESIAN_POINT('Origin',(0.,-0.64,-2.77555756156289E-17));
#11980=CARTESIAN_POINT('',(0.,0.,0.));
#11981=CARTESIAN_POINT('',(0.,0.,0.));
#11982=CARTESIAN_POINT('',(0.,0.,0.));
#11983=CARTESIAN_POINT('',(0.,0.,0.));
#11984=CARTESIAN_POINT('',(0.,0.,0.));
#11985=CARTESIAN_POINT('',(0.,0.,0.));
#11986=CARTESIAN_POINT('',(0.,0.,0.));
#11987=CARTESIAN_POINT('',(0.,0.,0.));
#11988=CARTESIAN_POINT('',(0.,0.,0.));
#11989=CARTESIAN_POINT('',(0.,0.,0.));
#11990=CARTESIAN_POINT('',(0.,0.,0.));
#11991=CARTESIAN_POINT('',(-8.5,-1.4,1.8));
#11992=CARTESIAN_POINT('',(-8.5,1.4,1.8));
#11993=CARTESIAN_POINT('',(-6.,-1.4,1.8));
#11994=CARTESIAN_POINT('',(-6.,1.4,1.8));
#11995=CARTESIAN_POINT('',(-4.,0.,11.));
#11996=CARTESIAN_POINT('',(0.,0.,14.));
#11997=CARTESIAN_POINT('',(-2.76256313292354,-1.,12.2374368670765));
#11998=CARTESIAN_POINT('',(-5.23743686707646,-1.,12.2374368670765));
#11999=CARTESIAN_POINT('',(-5.23743686707646,-1.,9.76256313292354));
#12000=CARTESIAN_POINT('',(-2.76256313292354,-1.,9.76256313292354));
#12001=CARTESIAN_POINT('',(-2.76256313292354,1.,12.2374368670765));
#12002=CARTESIAN_POINT('',(-5.23743686707646,1.,12.2374368670765));
#12003=CARTESIAN_POINT('',(-5.23743686707646,1.,9.76256313292354));
#12004=CARTESIAN_POINT('',(-2.76256313292354,1.,9.76256313292354));
#12005=CARTESIAN_POINT('',(1.13137084989848,1.13137084989848,16.9));
#12006=CARTESIAN_POINT('',(-1.13137084989848,1.13137084989848,16.9));
#12007=CARTESIAN_POINT('',(-1.13137084989848,-1.13137084989848,16.9));
#12008=CARTESIAN_POINT('',(1.13137084989848,-1.13137084989848,16.9));
#12009=CARTESIAN_POINT('',(-1.5,-4.5,0.));
#12010=CARTESIAN_POINT('',(-1.5,2.,0.));
#12011=CARTESIAN_POINT('',(1.5,-4.5,0.));
#12012=CARTESIAN_POINT('',(1.5,2.,0.));
#12013=CARTESIAN_POINT('',(-5.25982293614231,0.8,14.8604204653858));
#12014=CARTESIAN_POINT('',(0.,0.,0.));
#12015=CARTESIAN_POINT('',(0.,0.,0.));
#12016=CARTESIAN_POINT('',(0.,0.,0.));
#12017=CARTESIAN_POINT('',(0.,0.,0.));
#12018=CARTESIAN_POINT('',(0.,0.,0.));
#12019=CARTESIAN_POINT('',(0.,0.,0.));
#12020=CARTESIAN_POINT('',(0.,0.,0.));
#12021=CARTESIAN_POINT('',(0.,0.,0.));
#12022=CARTESIAN_POINT('',(-3.1,1.4,11.));
#12023=CARTESIAN_POINT('',(-2.82632109303527,-5.9,8.79263101785268));
#12024=CARTESIAN_POINT('',(-2.82632109303527,-2.5,8.79263101785268));
#12025=CARTESIAN_POINT('',(0.,0.,0.));
#12026=CARTESIAN_POINT('',(0.,0.,0.));
#12027=CARTESIAN_POINT('Origin',(-2.82632109303527,-5.6,8.79263101785268));
#12028=CARTESIAN_POINT('',(-3.32632109303527,-5.5,8.79263101785268));
#12029=CARTESIAN_POINT('Origin',(-2.82632109303527,-5.5,8.79263101785268));
#12030=CARTESIAN_POINT('',(-3.32632109303527,-4.7,8.79263101785268));
#12031=CARTESIAN_POINT('',(-3.32632109303527,-5.6,8.79263101785268));
#12032=CARTESIAN_POINT('Origin',(-2.82632109303527,-4.7,8.79263101785268));
#12033=CARTESIAN_POINT('Origin',(0.,-5.6,4.668081457105));
#12034=CARTESIAN_POINT('',(-0.5,-5.5,4.668081457105));
#12035=CARTESIAN_POINT('Origin',(0.,-5.5,4.668081457105));
#12036=CARTESIAN_POINT('',(-0.5,-4.7,4.668081457105));
#12037=CARTESIAN_POINT('',(-0.5,-5.6,4.668081457105));
#12038=CARTESIAN_POINT('Origin',(0.,-4.7,4.668081457105));
#12039=CARTESIAN_POINT('Origin',(0.,-5.5,4.668081457105));
#12040=CARTESIAN_POINT('',(-0.765462347451497,-4.7,4.90060542282476));
#12041=CARTESIAN_POINT('',(-0.765462347451497,-5.5,4.90060542282476));
#12042=CARTESIAN_POINT('',(-0.765462347451497,-5.5,4.90060542282476));
#12043=CARTESIAN_POINT('',(0.059447564698039,-4.7,5.46586964143181));
#12044=CARTESIAN_POINT('Origin',(0.,-4.7,4.668081457105));
#12045=CARTESIAN_POINT('',(0.059447564698039,-5.5,5.46586964143181));
#12046=CARTESIAN_POINT('',(0.059447564698039,-5.5,5.46586964143181));
#12047=CARTESIAN_POINT('Origin',(0.,-5.5,4.668081457105));
#12048=CARTESIAN_POINT('Origin',(-0.412454956074768,-5.5,4.38544934780147));
#12049=CARTESIAN_POINT('',(-2.88576865773331,-5.5,7.99484283352587));
#12050=CARTESIAN_POINT('',(-0.412454956074768,-5.5,4.38544934780147));
#12051=CARTESIAN_POINT('',(-2.88576865773331,-4.7,7.99484283352587));
#12052=CARTESIAN_POINT('',(-2.88576865773331,-5.5,7.99484283352587));
#12053=CARTESIAN_POINT('',(-0.412454956074768,-4.7,4.38544934780147));
#12054=CARTESIAN_POINT('Origin',(-2.82632109303527,-5.5,8.79263101785268));
#12055=CARTESIAN_POINT('',(-2.06085874558378,-5.5,8.56010705213293));
#12056=CARTESIAN_POINT('',(-2.4138661369605,-5.5,9.07526312715621));
#12057=CARTESIAN_POINT('Origin',(-2.82632109303527,-5.5,8.79263101785268));
#12058=CARTESIAN_POINT('Origin',(-2.4138661369605,-5.5,9.07526312715621));
#12059=CARTESIAN_POINT('',(-2.06085874558378,-4.7,8.56010705213293));
#12060=CARTESIAN_POINT('',(-2.4138661369605,-4.7,9.07526312715621));
#12061=CARTESIAN_POINT('',(-2.06085874558378,-5.5,8.56010705213293));
#12062=CARTESIAN_POINT('Origin',(-2.82632109303527,-5.5,8.79263101785268));
#12063=CARTESIAN_POINT('Origin',(-2.82632109303527,-4.7,8.79263101785268));
#12064=CARTESIAN_POINT('Origin',(-2.82632109303527,-4.7,8.79263101785268));
#12065=CARTESIAN_POINT('',(0.,0.,0.));
#12066=CARTESIAN_POINT('Origin',(-2.82632109303527,-5.5,8.79263101785268));
#12067=CARTESIAN_POINT('',(-3.13132109303527,-4.7,8.79263101785268));
#12068=CARTESIAN_POINT('Origin',(-2.82632109303527,-4.7,8.79263101785268));
#12069=CARTESIAN_POINT('',(-3.13132109303527,-5.5,8.79263101785268));
#12070=CARTESIAN_POINT('',(-3.13132109303527,-5.5,8.79263101785268));
#12071=CARTESIAN_POINT('Origin',(-2.82632109303527,-5.5,8.79263101785268));
#12072=CARTESIAN_POINT('Origin',(-2.82632109303527,-5.5,8.79263101785268));
#12073=CARTESIAN_POINT('',(-3.32632109303527,-4.7,8.79263101785268));
#12074=CARTESIAN_POINT('Origin',(-2.82632109303527,-4.7,8.79263101785268));
#12075=CARTESIAN_POINT('',(-3.32632109303527,-5.5,8.79263101785268));
#12076=CARTESIAN_POINT('',(-3.32632109303527,-5.5,8.79263101785268));
#12077=CARTESIAN_POINT('Origin',(-2.82632109303527,-5.5,8.79263101785268));
#12078=CARTESIAN_POINT('Origin',(-2.82632109303527,-4.7,8.79263101785268));
#12079=CARTESIAN_POINT('Origin',(-2.82632109303527,-5.5,8.79263101785268));
#12080=CARTESIAN_POINT('',(0.,0.,0.));
#12081=CARTESIAN_POINT('Origin',(0.,-5.5,4.668081457105));
#12082=CARTESIAN_POINT('',(-0.305,-4.7,4.668081457105));
#12083=CARTESIAN_POINT('Origin',(0.,-4.7,4.668081457105));
#12084=CARTESIAN_POINT('',(-0.305,-5.5,4.668081457105));
#12085=CARTESIAN_POINT('',(-0.305,-5.5,4.668081457105));
#12086=CARTESIAN_POINT('Origin',(0.,-5.5,4.668081457105));
#12087=CARTESIAN_POINT('Origin',(0.,-5.5,4.668081457105));
#12088=CARTESIAN_POINT('',(-0.5,-4.7,4.668081457105));
#12089=CARTESIAN_POINT('Origin',(0.,-4.7,4.668081457105));
#12090=CARTESIAN_POINT('',(-0.5,-5.5,4.668081457105));
#12091=CARTESIAN_POINT('',(-0.5,-5.5,4.668081457105));
#12092=CARTESIAN_POINT('Origin',(0.,-5.5,4.668081457105));
#12093=CARTESIAN_POINT('Origin',(0.,-4.7,4.668081457105));
#12094=CARTESIAN_POINT('Origin',(0.,-5.5,4.668081457105));
#12095=CARTESIAN_POINT('',(0.,0.,0.));
#12096=CARTESIAN_POINT('',(0.,0.,0.));
#12097=CARTESIAN_POINT('',(0.,0.,0.));
#12098=CARTESIAN_POINT('',(0.,0.,0.));
#12099=CARTESIAN_POINT('',(0.,0.,0.));
#12100=CARTESIAN_POINT('Origin',(0.,-6.1,4.668081457105));
#12101=CARTESIAN_POINT('',(-0.305,-4.69,4.668081457105));
#12102=CARTESIAN_POINT('Origin',(0.,-4.69,4.668081457105));
#12103=CARTESIAN_POINT('',(-0.305,-3.8,4.668081457105));
#12104=CARTESIAN_POINT('',(-0.305,-6.1,4.668081457105));
#12105=CARTESIAN_POINT('Origin',(0.,-3.8,4.668081457105));
#12106=CARTESIAN_POINT('Origin',(0.,-3.8,4.668081457105));
#12107=CARTESIAN_POINT('Origin',(0.,-4.69,4.668081457105));
#12108=CARTESIAN_POINT('',(-0.8,-4.69,4.16808146));
#12109=CARTESIAN_POINT('',(-0.8,-4.69,5.16808146));
#12110=CARTESIAN_POINT('',(-0.8,-4.69,4.4180814585525));
#12111=CARTESIAN_POINT('',(0.8,-4.69,4.16808146));
#12112=CARTESIAN_POINT('',(0.,-4.69,4.16808146));
#12113=CARTESIAN_POINT('',(0.8,-4.69,5.16808146));
#12114=CARTESIAN_POINT('',(0.8,-4.69,4.4180814585525));
#12115=CARTESIAN_POINT('',(0.,-4.69,5.16808146));
#12116=CARTESIAN_POINT('Origin',(0.8,-6.,4.16808146));
#12117=CARTESIAN_POINT('',(0.8,-0.894427190999916,4.16808146));
#12118=CARTESIAN_POINT('',(0.8,-6.,4.16808146));
#12119=CARTESIAN_POINT('',(0.8,-0.894427190999916,4.36808146));
#12120=CARTESIAN_POINT('',(0.8,-0.894427190999916,3.4));
#12121=CARTESIAN_POINT('',(0.8,0.,4.36808146));
#12122=CARTESIAN_POINT('',(0.8,-3.,4.36808146));
#12123=CARTESIAN_POINT('',(0.8,0.,5.16808146));
#12124=CARTESIAN_POINT('',(0.8,0.,4.16808146));
#12125=CARTESIAN_POINT('',(0.8,-6.,5.16808146));
#12126=CARTESIAN_POINT('Origin',(0.,-3.,4.16808146));
#12127=CARTESIAN_POINT('',(-0.8,-0.894427190999916,4.16808146));
#12128=CARTESIAN_POINT('',(-0.8,0.,4.16808146));
#12129=CARTESIAN_POINT('Origin',(0.,0.,4.16808146));
#12130=CARTESIAN_POINT('Origin',(-0.8,0.,4.16808146));
#12131=CARTESIAN_POINT('',(-0.8,0.,5.16808146));
#12132=CARTESIAN_POINT('',(-0.8,0.,5.16808146));
#12133=CARTESIAN_POINT('',(-0.8,0.,4.36808146));
#12134=CARTESIAN_POINT('',(-0.8,0.,4.16808146));
#12135=CARTESIAN_POINT('',(-0.8,-0.894427190999916,4.36808146));
#12136=CARTESIAN_POINT('',(-0.8,0.,4.36808146));
#12137=CARTESIAN_POINT('',(-0.8,-0.894427190999916,3.4));
#12138=CARTESIAN_POINT('Origin',(0.8,0.,4.16808146));
#12139=CARTESIAN_POINT('',(0.6,0.,5.16808146));
#12140=CARTESIAN_POINT('',(0.6,0.,4.36808146));
#12141=CARTESIAN_POINT('',(0.6,0.,4.36808146));
#12142=CARTESIAN_POINT('',(0.8,0.,5.16808146));
#12143=CARTESIAN_POINT('',(0.4,0.,4.36808146));
#12144=CARTESIAN_POINT('Origin',(0.8,0.,4.16808146));
#12145=CARTESIAN_POINT('',(-0.6,-7.34788079488412E-17,4.36808146));
#12146=CARTESIAN_POINT('',(0.4,0.,4.36808146));
#12147=CARTESIAN_POINT('',(-0.6,0.,5.16808146));
#12148=CARTESIAN_POINT('',(0.8,0.,5.16808146));
#12149=CARTESIAN_POINT('',(-0.6,0.,4.36808146));
#12150=CARTESIAN_POINT('Origin',(0.,-3.,5.16808146));
#12151=CARTESIAN_POINT('Origin',(0.,0.,5.16808146));
#12152=CARTESIAN_POINT('Origin',(0.,0.,4.36808146));
#12153=CARTESIAN_POINT('',(-0.6,-7.34788079488412E-17,19.));
#12154=CARTESIAN_POINT('Origin',(0.,0.,19.));
#12155=CARTESIAN_POINT('',(-0.6,-7.34788079488412E-17,4.36808146));
#12156=CARTESIAN_POINT('Origin',(0.,0.,4.36808146));
#12157=CARTESIAN_POINT('Origin',(0.,0.,4.36808146));
#12158=CARTESIAN_POINT('',(-1.2,-1.46957615897682E-16,4.36808146));
#12159=CARTESIAN_POINT('Origin',(0.,0.,4.36808146));
#12160=CARTESIAN_POINT('Origin',(0.,0.,4.36808146));
#12161=CARTESIAN_POINT('Origin',(0.,0.,3.4));
#12162=CARTESIAN_POINT('',(-1.2,-1.46957615897682E-16,3.4));
#12163=CARTESIAN_POINT('',(-1.2,-1.46957615897682E-16,3.4));
#12164=CARTESIAN_POINT('Origin',(0.,0.,3.4));
#12165=CARTESIAN_POINT('Origin',(0.,0.,3.4));
#12166=CARTESIAN_POINT('Origin',(0.,0.,19.));
#12167=CARTESIAN_POINT('Origin',(0.29,-5.75,4.668081457105));
#12168=CARTESIAN_POINT('',(0.29,-5.88527749258469,4.57360923896654));
#12169=CARTESIAN_POINT('',(0.29,-5.61472250741531,4.57360923896654));
#12170=CARTESIAN_POINT('',(0.29,-6.1,4.57360923896654));
#12171=CARTESIAN_POINT('Origin',(0.29,-5.75,4.668081457105));
#12172=CARTESIAN_POINT('Origin',(0.29,-5.75,4.668081457105));
#12173=CARTESIAN_POINT('',(0.29,-5.88527749258469,4.76255367524346));
#12174=CARTESIAN_POINT('Ctrl Pts',(0.29,-5.88527749258469,4.76255367524346));
#12175=CARTESIAN_POINT('Ctrl Pts',(0.293078111442152,-5.89187616839667,
4.75310484112255));
#12176=CARTESIAN_POINT('Ctrl Pts',(0.295928845896546,-5.89761208817693,
4.7427508396533));
#12177=CARTESIAN_POINT('Ctrl Pts',(0.302593996394854,-5.91067507972101,
4.71157336496124));
#12178=CARTESIAN_POINT('Ctrl Pts',(0.305,-5.915,4.6892669703376));
#12179=CARTESIAN_POINT('Ctrl Pts',(0.305,-5.915,4.6468959438724));
#12180=CARTESIAN_POINT('Ctrl Pts',(0.302593996394854,-5.91067507972101,
4.62458954924876));
#12181=CARTESIAN_POINT('Ctrl Pts',(0.295928845896546,-5.89761208817693,
4.5934120745567));
#12182=CARTESIAN_POINT('Ctrl Pts',(0.293078111442152,-5.89187616839667,
4.58305807308745));
#12183=CARTESIAN_POINT('Ctrl Pts',(0.29,-5.88527749258469,4.57360923896654));
#12184=CARTESIAN_POINT('',(0.29,-5.75,4.833081457105));
#12185=CARTESIAN_POINT('Origin',(0.29,-5.75,4.668081457105));
#12186=CARTESIAN_POINT('',(0.8,-5.75,4.833081457105));
#12187=CARTESIAN_POINT('',(0.29,-5.75,4.833081457105));
#12188=CARTESIAN_POINT('Origin',(0.8,-5.75,4.668081457105));
#12189=CARTESIAN_POINT('',(0.29,-5.61472250741531,4.76255367524346));
#12190=CARTESIAN_POINT('Origin',(0.29,-5.75,4.668081457105));
#12191=CARTESIAN_POINT('Ctrl Pts',(0.29,-5.61472250741531,4.57360923896654));
#12192=CARTESIAN_POINT('Ctrl Pts',(0.293078111442152,-5.60812383160333,
4.58305807308745));
#12193=CARTESIAN_POINT('Ctrl Pts',(0.295928845896546,-5.60238791182307,
4.5934120745567));
#12194=CARTESIAN_POINT('Ctrl Pts',(0.302593996394854,-5.58932492027899,
4.62458954924876));
#12195=CARTESIAN_POINT('Ctrl Pts',(0.305,-5.585,4.6468959438724));
#12196=CARTESIAN_POINT('Ctrl Pts',(0.305,-5.585,4.6892669703376));
#12197=CARTESIAN_POINT('Ctrl Pts',(0.302593996394854,-5.58932492027899,
4.71157336496124));
#12198=CARTESIAN_POINT('Ctrl Pts',(0.295928845896546,-5.60238791182307,
4.7427508396533));
#12199=CARTESIAN_POINT('Ctrl Pts',(0.293078111442152,-5.60812383160333,
4.75310484112255));
#12200=CARTESIAN_POINT('Ctrl Pts',(0.29,-5.61472250741531,4.76255367524346));
#12201=CARTESIAN_POINT('Origin',(0.29,-5.75,4.668081457105));
#12202=CARTESIAN_POINT('',(0.29,-6.1,4.76255367524346));
#12203=CARTESIAN_POINT('Origin',(0.,-6.1,4.668081457105));
#12204=CARTESIAN_POINT('',(-0.305,-6.,4.668081457105));
#12205=CARTESIAN_POINT('Origin',(0.,-6.,4.668081457105));
#12206=CARTESIAN_POINT('',(-0.305,-5.51,4.668081457105));
#12207=CARTESIAN_POINT('',(-0.305,-6.1,4.668081457105));
#12208=CARTESIAN_POINT('Origin',(0.,-5.51,4.668081457105));
#12209=CARTESIAN_POINT('Origin',(-0.8,-6.,4.16808146));
#12210=CARTESIAN_POINT('',(-0.8,-6.,4.16808146));
#12211=CARTESIAN_POINT('',(0.8,-6.,4.16808146));
#12212=CARTESIAN_POINT('',(-0.8,-6.,4.16808146));
#12213=CARTESIAN_POINT('',(0.8,-6.,5.16808146));
#12214=CARTESIAN_POINT('',(0.8,-6.,4.16808146));
#12215=CARTESIAN_POINT('',(-0.8,-6.,5.16808146));
#12216=CARTESIAN_POINT('',(-0.8,-6.,5.16808146));
#12217=CARTESIAN_POINT('',(-0.8,-6.,4.16808146));
#12218=CARTESIAN_POINT('Origin',(-0.8,0.,4.16808146));
#12219=CARTESIAN_POINT('',(-0.8,-5.51,5.16808146));
#12220=CARTESIAN_POINT('',(-0.8,-5.51,4.16808146));
#12221=CARTESIAN_POINT('',(-0.8,-5.51,4.4180814585525));
#12222=CARTESIAN_POINT('',(-0.8,0.,4.16808146));
#12223=CARTESIAN_POINT('',(-0.8,0.,5.16808146));
#12224=CARTESIAN_POINT('Origin',(0.,-3.,5.16808146));
#12225=CARTESIAN_POINT('',(0.8,-5.51,5.16808146));
#12226=CARTESIAN_POINT('',(0.,-5.51,5.16808146));
#12227=CARTESIAN_POINT('',(0.8,-6.,5.16808146));
#12228=CARTESIAN_POINT('Origin',(0.,-3.,4.16808146));
#12229=CARTESIAN_POINT('',(0.8,-5.51,4.16808146));
#12230=CARTESIAN_POINT('',(0.,-5.51,4.16808146));
#12231=CARTESIAN_POINT('',(0.8,-6.,4.16808146));
#12232=CARTESIAN_POINT('Origin',(0.8,-6.,4.16808146));
#12233=CARTESIAN_POINT('',(0.8,-5.51,4.4180814585525));
#12234=CARTESIAN_POINT('Origin',(0.,-5.51,4.668081457105));
#12235=CARTESIAN_POINT('',(0.,0.,0.));
#12236=CARTESIAN_POINT('Origin',(0.,-6.,4.668081457105));
#12237=CARTESIAN_POINT('',(-0.5,-6.,4.668081457105));
#12238=CARTESIAN_POINT('Origin',(0.,-6.,4.668081457105));
#12239=CARTESIAN_POINT('',(-0.3,-6.,4.668081457105));
#12240=CARTESIAN_POINT('Origin',(0.,-6.,4.668081457105));
#12241=CARTESIAN_POINT('Origin',(0.,-6.2,4.668081457105));
#12242=CARTESIAN_POINT('',(-0.5,-6.2,4.668081457105));
#12243=CARTESIAN_POINT('',(-0.5,-6.2,4.668081457105));
#12244=CARTESIAN_POINT('Origin',(0.,-6.2,4.668081457105));
#12245=CARTESIAN_POINT('Origin',(0.,-6.2,4.668081457105));
#12246=CARTESIAN_POINT('Origin',(0.,-6.,4.668081457105));
#12247=CARTESIAN_POINT('',(-0.3,-3.9,4.668081457105));
#12248=CARTESIAN_POINT('Origin',(0.,-3.9,4.668081457105));
#12249=CARTESIAN_POINT('',(-0.3,-6.,4.668081457105));
#12250=CARTESIAN_POINT('Origin',(0.,-3.9,4.668081457105));
#12251=CARTESIAN_POINT('',(0.,0.,0.));
#12252=CARTESIAN_POINT('Origin',(0.,0.,3.));
#12253=CARTESIAN_POINT('',(-1.,-1.22464679914735E-16,3.4));
#12254=CARTESIAN_POINT('Origin',(0.,0.,3.4));
#12255=CARTESIAN_POINT('',(-1.,-1.22464679914735E-16,3.));
#12256=CARTESIAN_POINT('',(-1.,-1.22464679914735E-16,3.));
#12257=CARTESIAN_POINT('Origin',(0.,0.,3.));
#12258=CARTESIAN_POINT('Origin',(0.,0.,3.4));
#12259=CARTESIAN_POINT('Origin',(0.,0.,3.));
#12260=CARTESIAN_POINT('',(0.,0.,0.));
#12261=CARTESIAN_POINT('Origin',(0.0577350269189626,0.,-0.1));
#12262=CARTESIAN_POINT('',(0.0577350269189626,0.,-0.1));
#12263=CARTESIAN_POINT('',(0.115470053837925,0.,0.));
#12264=CARTESIAN_POINT('',(0.0934187836487032,0.,-0.0381939203391614));
#12265=CARTESIAN_POINT('',(0.0577350269189626,-0.2,-0.1));
#12266=CARTESIAN_POINT('',(0.0577350269189626,0.,-0.1));
#12267=CARTESIAN_POINT('',(0.115470053837925,-0.2,0.));
#12268=CARTESIAN_POINT('',(0.115470053837925,-0.2,0.));
#12269=CARTESIAN_POINT('',(0.115470053837925,0.,0.));
#12270=CARTESIAN_POINT('Origin',(-0.0577350269189626,0.,-0.1));
#12271=CARTESIAN_POINT('',(-0.0577350269189626,0.,-0.1));
#12272=CARTESIAN_POINT('',(0.0561324865405187,0.,-0.1));
#12273=CARTESIAN_POINT('',(-0.0577350269189626,-0.2,-0.1));
#12274=CARTESIAN_POINT('',(-0.0577350269189626,0.,-0.1));
#12275=CARTESIAN_POINT('',(0.0577350269189626,-0.2,-0.1));
#12276=CARTESIAN_POINT('Origin',(-0.115470053837925,0.,-1.38777878078145E-17));
#12277=CARTESIAN_POINT('',(-0.115470053837925,0.,-1.41410031829988E-17));
#12278=CARTESIAN_POINT('',(-0.0797862971081845,0.,-0.0618060796608387));
#12279=CARTESIAN_POINT('',(-0.115470053837925,-0.2,-1.38777878078145E-17));
#12280=CARTESIAN_POINT('',(-0.115470053837925,0.,-1.41410031829988E-17));
#12281=CARTESIAN_POINT('',(-0.0577350269189626,-0.2,-0.1));
#12282=CARTESIAN_POINT('Origin',(-0.0577350269189626,0.,0.1));
#12283=CARTESIAN_POINT('',(-0.0577350269189626,0.,0.1));
#12284=CARTESIAN_POINT('',(-0.0509187836487033,0.,0.111806079660839));
#12285=CARTESIAN_POINT('',(-0.0577350269189626,-0.2,0.1));
#12286=CARTESIAN_POINT('',(-0.0577350269189626,0.,0.1));
#12287=CARTESIAN_POINT('',(-0.115470053837925,-0.2,-1.41410031829988E-17));
#12288=CARTESIAN_POINT('Origin',(0.0577350269189626,0.,0.1));
#12289=CARTESIAN_POINT('',(0.0577350269189626,0.,0.1));
#12290=CARTESIAN_POINT('',(0.113867513459481,0.,0.1));
#12291=CARTESIAN_POINT('',(0.0577350269189626,-0.2,0.1));
#12292=CARTESIAN_POINT('',(0.0577350269189626,0.,0.1));
#12293=CARTESIAN_POINT('',(-0.0577350269189626,-0.2,0.1));
#12294=CARTESIAN_POINT('Origin',(0.115470053837925,0.,0.));
#12295=CARTESIAN_POINT('',(0.122286297108185,0.,-0.0118060796608386));
#12296=CARTESIAN_POINT('',(0.0577350269189626,-0.2,0.1));
#12297=CARTESIAN_POINT('Origin',(0.,-0.2,0.));
#12298=CARTESIAN_POINT('Origin',(0.17,0.,0.));
#12299=CARTESIAN_POINT('',(-0.17,-8.67361737988404E-18,-2.0818995585505E-17));
#12300=CARTESIAN_POINT('Origin',(0.,0.,0.));
#12301=CARTESIAN_POINT('Origin',(0.,-0.015,0.));
#12302=CARTESIAN_POINT('',(-0.1954,-0.0254,-2.39295984553393E-17));
#12303=CARTESIAN_POINT('Origin',(0.,-0.0254,0.));
#12304=CARTESIAN_POINT('',(-0.185,-0.015,-2.2655965784226E-17));
#12305=CARTESIAN_POINT('Origin',(0.,-0.2775,0.));
#12306=CARTESIAN_POINT('',(-0.1954,-0.5296,2.39295984553393E-17));
#12307=CARTESIAN_POINT('Origin',(0.,-0.5296,0.));
#12308=CARTESIAN_POINT('',(-0.1954,-0.2775,-2.39295984553393E-17));
#12309=CARTESIAN_POINT('Origin',(0.,-0.5625,0.));
#12310=CARTESIAN_POINT('',(-0.125,-0.6,-1.53080849893419E-17));
#12311=CARTESIAN_POINT('Origin',(0.,-0.6,0.));
#12312=CARTESIAN_POINT('',(-0.1625,-0.5625,-1.99005104861445E-17));
#12313=CARTESIAN_POINT('Origin',(0.,-0.6,0.));
#12314=CARTESIAN_POINT('',(0.,0.,0.));
#12315=CARTESIAN_POINT('',(0.,0.,0.));
#12316=CARTESIAN_POINT('',(0.,0.,0.));
#12317=CARTESIAN_POINT('',(0.9,-5.75,4.668081457105));
#12318=CARTESIAN_POINT('',(0.,0.,0.));
#12319=CARTESIAN_POINT('',(0.,0.,0.));
#12320=CARTESIAN_POINT('',(0.,0.,0.));
#12321=CARTESIAN_POINT('',(0.,0.,0.));
#12322=UNCERTAINTY_MEASURE_WITH_UNIT(LENGTH_MEASURE(0.001),#12414,
'DISTANCE_ACCURACY_VALUE',
'Maximum model space distance between geometric entities at asserted c
onnectivities');
#12323=UNCERTAINTY_MEASURE_WITH_UNIT(LENGTH_MEASURE(0.001),#12414,
'DISTANCE_ACCURACY_VALUE',
'Maximum model space distance between geometric entities at asserted c
onnectivities');
#12324=UNCERTAINTY_MEASURE_WITH_UNIT(LENGTH_MEASURE(0.001),#12414,
'DISTANCE_ACCURACY_VALUE',
'Maximum model space distance between geometric entities at asserted c
onnectivities');
#12325=UNCERTAINTY_MEASURE_WITH_UNIT(LENGTH_MEASURE(0.001),#12414,
'DISTANCE_ACCURACY_VALUE',
'Maximum model space distance between geometric entities at asserted c
onnectivities');
#12326=UNCERTAINTY_MEASURE_WITH_UNIT(LENGTH_MEASURE(0.001),#12414,
'DISTANCE_ACCURACY_VALUE',
'Maximum model space distance between geometric entities at asserted c
onnectivities');
#12327=UNCERTAINTY_MEASURE_WITH_UNIT(LENGTH_MEASURE(0.001),#12414,
'DISTANCE_ACCURACY_VALUE',
'Maximum model space distance between geometric entities at asserted c
onnectivities');
#12328=UNCERTAINTY_MEASURE_WITH_UNIT(LENGTH_MEASURE(0.001),#12414,
'DISTANCE_ACCURACY_VALUE',
'Maximum model space distance between geometric entities at asserted c
onnectivities');
#12329=UNCERTAINTY_MEASURE_WITH_UNIT(LENGTH_MEASURE(0.001),#12414,
'DISTANCE_ACCURACY_VALUE',
'Maximum model space distance between geometric entities at asserted c
onnectivities');
#12330=UNCERTAINTY_MEASURE_WITH_UNIT(LENGTH_MEASURE(0.001),#12414,
'DISTANCE_ACCURACY_VALUE',
'Maximum model space distance between geometric entities at asserted c
onnectivities');
#12331=UNCERTAINTY_MEASURE_WITH_UNIT(LENGTH_MEASURE(0.001),#12414,
'DISTANCE_ACCURACY_VALUE',
'Maximum model space distance between geometric entities at asserted c
onnectivities');
#12332=UNCERTAINTY_MEASURE_WITH_UNIT(LENGTH_MEASURE(0.001),#12414,
'DISTANCE_ACCURACY_VALUE',
'Maximum model space distance between geometric entities at asserted c
onnectivities');
#12333=UNCERTAINTY_MEASURE_WITH_UNIT(LENGTH_MEASURE(0.001),#12414,
'DISTANCE_ACCURACY_VALUE',
'Maximum model space distance between geometric entities at asserted c
onnectivities');
#12334=UNCERTAINTY_MEASURE_WITH_UNIT(LENGTH_MEASURE(0.001),#12414,
'DISTANCE_ACCURACY_VALUE',
'Maximum model space distance between geometric entities at asserted c
onnectivities');
#12335=UNCERTAINTY_MEASURE_WITH_UNIT(LENGTH_MEASURE(0.001),#12414,
'DISTANCE_ACCURACY_VALUE',
'Maximum model space distance between geometric entities at asserted c
onnectivities');
#12336=UNCERTAINTY_MEASURE_WITH_UNIT(LENGTH_MEASURE(0.001),#12414,
'DISTANCE_ACCURACY_VALUE',
'Maximum model space distance between geometric entities at asserted c
onnectivities');
#12337=UNCERTAINTY_MEASURE_WITH_UNIT(LENGTH_MEASURE(0.001),#12414,
'DISTANCE_ACCURACY_VALUE',
'Maximum model space distance between geometric entities at asserted c
onnectivities');
#12338=UNCERTAINTY_MEASURE_WITH_UNIT(LENGTH_MEASURE(0.001),#12414,
'DISTANCE_ACCURACY_VALUE',
'Maximum model space distance between geometric entities at asserted c
onnectivities');
#12339=UNCERTAINTY_MEASURE_WITH_UNIT(LENGTH_MEASURE(0.001),#12414,
'DISTANCE_ACCURACY_VALUE',
'Maximum model space distance between geometric entities at asserted c
onnectivities');
#12340=UNCERTAINTY_MEASURE_WITH_UNIT(LENGTH_MEASURE(0.001),#12414,
'DISTANCE_ACCURACY_VALUE',
'Maximum model space distance between geometric entities at asserted c
onnectivities');
#12341=UNCERTAINTY_MEASURE_WITH_UNIT(LENGTH_MEASURE(0.001),#12414,
'DISTANCE_ACCURACY_VALUE',
'Maximum model space distance between geometric entities at asserted c
onnectivities');
#12342=UNCERTAINTY_MEASURE_WITH_UNIT(LENGTH_MEASURE(0.001),#12414,
'DISTANCE_ACCURACY_VALUE',
'Maximum model space distance between geometric entities at asserted c
onnectivities');
#12343=UNCERTAINTY_MEASURE_WITH_UNIT(LENGTH_MEASURE(0.001),#12414,
'DISTANCE_ACCURACY_VALUE',
'Maximum model space distance between geometric entities at asserted c
onnectivities');
#12344=UNCERTAINTY_MEASURE_WITH_UNIT(LENGTH_MEASURE(0.001),#12414,
'DISTANCE_ACCURACY_VALUE',
'Maximum model space distance between geometric entities at asserted c
onnectivities');
#12345=UNCERTAINTY_MEASURE_WITH_UNIT(LENGTH_MEASURE(0.001),#12414,
'DISTANCE_ACCURACY_VALUE',
'Maximum model space distance between geometric entities at asserted c
onnectivities');
#12346=UNCERTAINTY_MEASURE_WITH_UNIT(LENGTH_MEASURE(0.001),#12414,
'DISTANCE_ACCURACY_VALUE',
'Maximum model space distance between geometric entities at asserted c
onnectivities');
#12347=UNCERTAINTY_MEASURE_WITH_UNIT(LENGTH_MEASURE(0.001),#12414,
'DISTANCE_ACCURACY_VALUE',
'Maximum model space distance between geometric entities at asserted c
onnectivities');
#12348=UNCERTAINTY_MEASURE_WITH_UNIT(LENGTH_MEASURE(0.001),#12414,
'DISTANCE_ACCURACY_VALUE',
'Maximum model space distance between geometric entities at asserted c
onnectivities');
#12349=UNCERTAINTY_MEASURE_WITH_UNIT(LENGTH_MEASURE(0.001),#12414,
'DISTANCE_ACCURACY_VALUE',
'Maximum model space distance between geometric entities at asserted c
onnectivities');
#12350=UNCERTAINTY_MEASURE_WITH_UNIT(LENGTH_MEASURE(0.001),#12414,
'DISTANCE_ACCURACY_VALUE',
'Maximum model space distance between geometric entities at asserted c
onnectivities');
#12351=UNCERTAINTY_MEASURE_WITH_UNIT(LENGTH_MEASURE(0.001),#12414,
'DISTANCE_ACCURACY_VALUE',
'Maximum model space distance between geometric entities at asserted c
onnectivities');
#12352=UNCERTAINTY_MEASURE_WITH_UNIT(LENGTH_MEASURE(0.001),#12414,
'DISTANCE_ACCURACY_VALUE',
'Maximum model space distance between geometric entities at asserted c
onnectivities');
#12353=UNCERTAINTY_MEASURE_WITH_UNIT(LENGTH_MEASURE(0.001),#12414,
'DISTANCE_ACCURACY_VALUE',
'Maximum model space distance between geometric entities at asserted c
onnectivities');
#12354=UNCERTAINTY_MEASURE_WITH_UNIT(LENGTH_MEASURE(0.001),#12414,
'DISTANCE_ACCURACY_VALUE',
'Maximum model space distance between geometric entities at asserted c
onnectivities');
#12355=UNCERTAINTY_MEASURE_WITH_UNIT(LENGTH_MEASURE(0.001),#12414,
'DISTANCE_ACCURACY_VALUE',
'Maximum model space distance between geometric entities at asserted c
onnectivities');
#12356=UNCERTAINTY_MEASURE_WITH_UNIT(LENGTH_MEASURE(0.001),#12414,
'DISTANCE_ACCURACY_VALUE',
'Maximum model space distance between geometric entities at asserted c
onnectivities');
#12357=UNCERTAINTY_MEASURE_WITH_UNIT(LENGTH_MEASURE(0.001),#12414,
'DISTANCE_ACCURACY_VALUE',
'Maximum model space distance between geometric entities at asserted c
onnectivities');
#12358=UNCERTAINTY_MEASURE_WITH_UNIT(LENGTH_MEASURE(0.001),#12414,
'DISTANCE_ACCURACY_VALUE',
'Maximum model space distance between geometric entities at asserted c
onnectivities');
#12359=UNCERTAINTY_MEASURE_WITH_UNIT(LENGTH_MEASURE(0.001),#12414,
'DISTANCE_ACCURACY_VALUE',
'Maximum model space distance between geometric entities at asserted c
onnectivities');
#12360=UNCERTAINTY_MEASURE_WITH_UNIT(LENGTH_MEASURE(0.001),#12414,
'DISTANCE_ACCURACY_VALUE',
'Maximum model space distance between geometric entities at asserted c
onnectivities');
#12361=UNCERTAINTY_MEASURE_WITH_UNIT(LENGTH_MEASURE(0.001),#12414,
'DISTANCE_ACCURACY_VALUE',
'Maximum model space distance between geometric entities at asserted c
onnectivities');
#12362=UNCERTAINTY_MEASURE_WITH_UNIT(LENGTH_MEASURE(0.001),#12414,
'DISTANCE_ACCURACY_VALUE',
'Maximum model space distance between geometric entities at asserted c
onnectivities');
#12363=UNCERTAINTY_MEASURE_WITH_UNIT(LENGTH_MEASURE(0.001),#12414,
'DISTANCE_ACCURACY_VALUE',
'Maximum model space distance between geometric entities at asserted c
onnectivities');
#12364=UNCERTAINTY_MEASURE_WITH_UNIT(LENGTH_MEASURE(0.001),#12414,
'DISTANCE_ACCURACY_VALUE',
'Maximum model space distance between geometric entities at asserted c
onnectivities');
#12365=UNCERTAINTY_MEASURE_WITH_UNIT(LENGTH_MEASURE(0.001),#12414,
'DISTANCE_ACCURACY_VALUE',
'Maximum model space distance between geometric entities at asserted c
onnectivities');
#12366=UNCERTAINTY_MEASURE_WITH_UNIT(LENGTH_MEASURE(0.001),#12414,
'DISTANCE_ACCURACY_VALUE',
'Maximum model space distance between geometric entities at asserted c
onnectivities');
#12367=UNCERTAINTY_MEASURE_WITH_UNIT(LENGTH_MEASURE(0.001),#12414,
'DISTANCE_ACCURACY_VALUE',
'Maximum model space distance between geometric entities at asserted c
onnectivities');
#12368=(
GEOMETRIC_REPRESENTATION_CONTEXT(3)
GLOBAL_UNCERTAINTY_ASSIGNED_CONTEXT((#12322))
GLOBAL_UNIT_ASSIGNED_CONTEXT((#12414,#12416,#12417))
REPRESENTATION_CONTEXT('','3D')
);
#12369=(
GEOMETRIC_REPRESENTATION_CONTEXT(3)
GLOBAL_UNCERTAINTY_ASSIGNED_CONTEXT((#12323))
GLOBAL_UNIT_ASSIGNED_CONTEXT((#12414,#12416,#12417))
REPRESENTATION_CONTEXT('','3D')
);
#12370=(
GEOMETRIC_REPRESENTATION_CONTEXT(3)
GLOBAL_UNCERTAINTY_ASSIGNED_CONTEXT((#12324))
GLOBAL_UNIT_ASSIGNED_CONTEXT((#12414,#12416,#12417))
REPRESENTATION_CONTEXT('','3D')
);
#12371=(
GEOMETRIC_REPRESENTATION_CONTEXT(3)
GLOBAL_UNCERTAINTY_ASSIGNED_CONTEXT((#12325))
GLOBAL_UNIT_ASSIGNED_CONTEXT((#12414,#12416,#12417))
REPRESENTATION_CONTEXT('','3D')
);
#12372=(
GEOMETRIC_REPRESENTATION_CONTEXT(3)
GLOBAL_UNCERTAINTY_ASSIGNED_CONTEXT((#12326))
GLOBAL_UNIT_ASSIGNED_CONTEXT((#12414,#12416,#12417))
REPRESENTATION_CONTEXT('','3D')
);
#12373=(
GEOMETRIC_REPRESENTATION_CONTEXT(3)
GLOBAL_UNCERTAINTY_ASSIGNED_CONTEXT((#12327))
GLOBAL_UNIT_ASSIGNED_CONTEXT((#12414,#12416,#12417))
REPRESENTATION_CONTEXT('','3D')
);
#12374=(
GEOMETRIC_REPRESENTATION_CONTEXT(3)
GLOBAL_UNCERTAINTY_ASSIGNED_CONTEXT((#12328))
GLOBAL_UNIT_ASSIGNED_CONTEXT((#12414,#12416,#12417))
REPRESENTATION_CONTEXT('','3D')
);
#12375=(
GEOMETRIC_REPRESENTATION_CONTEXT(3)
GLOBAL_UNCERTAINTY_ASSIGNED_CONTEXT((#12329))
GLOBAL_UNIT_ASSIGNED_CONTEXT((#12414,#12416,#12417))
REPRESENTATION_CONTEXT('','3D')
);
#12376=(
GEOMETRIC_REPRESENTATION_CONTEXT(3)
GLOBAL_UNCERTAINTY_ASSIGNED_CONTEXT((#12330))
GLOBAL_UNIT_ASSIGNED_CONTEXT((#12414,#12416,#12417))
REPRESENTATION_CONTEXT('','3D')
);
#12377=(
GEOMETRIC_REPRESENTATION_CONTEXT(3)
GLOBAL_UNCERTAINTY_ASSIGNED_CONTEXT((#12331))
GLOBAL_UNIT_ASSIGNED_CONTEXT((#12414,#12416,#12417))
REPRESENTATION_CONTEXT('','3D')
);
#12378=(
GEOMETRIC_REPRESENTATION_CONTEXT(3)
GLOBAL_UNCERTAINTY_ASSIGNED_CONTEXT((#12332))
GLOBAL_UNIT_ASSIGNED_CONTEXT((#12414,#12416,#12417))
REPRESENTATION_CONTEXT('','3D')
);
#12379=(
GEOMETRIC_REPRESENTATION_CONTEXT(3)
GLOBAL_UNCERTAINTY_ASSIGNED_CONTEXT((#12333))
GLOBAL_UNIT_ASSIGNED_CONTEXT((#12414,#12416,#12417))
REPRESENTATION_CONTEXT('','3D')
);
#12380=(
GEOMETRIC_REPRESENTATION_CONTEXT(3)
GLOBAL_UNCERTAINTY_ASSIGNED_CONTEXT((#12334))
GLOBAL_UNIT_ASSIGNED_CONTEXT((#12414,#12416,#12417))
REPRESENTATION_CONTEXT('','3D')
);
#12381=(
GEOMETRIC_REPRESENTATION_CONTEXT(3)
GLOBAL_UNCERTAINTY_ASSIGNED_CONTEXT((#12335))
GLOBAL_UNIT_ASSIGNED_CONTEXT((#12414,#12416,#12417))
REPRESENTATION_CONTEXT('','3D')
);
#12382=(
GEOMETRIC_REPRESENTATION_CONTEXT(3)
GLOBAL_UNCERTAINTY_ASSIGNED_CONTEXT((#12336))
GLOBAL_UNIT_ASSIGNED_CONTEXT((#12414,#12416,#12417))
REPRESENTATION_CONTEXT('','3D')
);
#12383=(
GEOMETRIC_REPRESENTATION_CONTEXT(3)
GLOBAL_UNCERTAINTY_ASSIGNED_CONTEXT((#12337))
GLOBAL_UNIT_ASSIGNED_CONTEXT((#12414,#12416,#12417))
REPRESENTATION_CONTEXT('','3D')
);
#12384=(
GEOMETRIC_REPRESENTATION_CONTEXT(3)
GLOBAL_UNCERTAINTY_ASSIGNED_CONTEXT((#12338))
GLOBAL_UNIT_ASSIGNED_CONTEXT((#12414,#12416,#12417))
REPRESENTATION_CONTEXT('','3D')
);
#12385=(
GEOMETRIC_REPRESENTATION_CONTEXT(3)
GLOBAL_UNCERTAINTY_ASSIGNED_CONTEXT((#12339))
GLOBAL_UNIT_ASSIGNED_CONTEXT((#12414,#12416,#12417))
REPRESENTATION_CONTEXT('','3D')
);
#12386=(
GEOMETRIC_REPRESENTATION_CONTEXT(3)
GLOBAL_UNCERTAINTY_ASSIGNED_CONTEXT((#12340))
GLOBAL_UNIT_ASSIGNED_CONTEXT((#12414,#12416,#12417))
REPRESENTATION_CONTEXT('','3D')
);
#12387=(
GEOMETRIC_REPRESENTATION_CONTEXT(3)
GLOBAL_UNCERTAINTY_ASSIGNED_CONTEXT((#12341))
GLOBAL_UNIT_ASSIGNED_CONTEXT((#12414,#12416,#12417))
REPRESENTATION_CONTEXT('','3D')
);
#12388=(
GEOMETRIC_REPRESENTATION_CONTEXT(3)
GLOBAL_UNCERTAINTY_ASSIGNED_CONTEXT((#12342))
GLOBAL_UNIT_ASSIGNED_CONTEXT((#12414,#12416,#12417))
REPRESENTATION_CONTEXT('','3D')
);
#12389=(
GEOMETRIC_REPRESENTATION_CONTEXT(3)
GLOBAL_UNCERTAINTY_ASSIGNED_CONTEXT((#12343))
GLOBAL_UNIT_ASSIGNED_CONTEXT((#12414,#12416,#12417))
REPRESENTATION_CONTEXT('','3D')
);
#12390=(
GEOMETRIC_REPRESENTATION_CONTEXT(3)
GLOBAL_UNCERTAINTY_ASSIGNED_CONTEXT((#12344))
GLOBAL_UNIT_ASSIGNED_CONTEXT((#12414,#12416,#12417))
REPRESENTATION_CONTEXT('','3D')
);
#12391=(
GEOMETRIC_REPRESENTATION_CONTEXT(3)
GLOBAL_UNCERTAINTY_ASSIGNED_CONTEXT((#12345))
GLOBAL_UNIT_ASSIGNED_CONTEXT((#12414,#12416,#12417))
REPRESENTATION_CONTEXT('','3D')
);
#12392=(
GEOMETRIC_REPRESENTATION_CONTEXT(3)
GLOBAL_UNCERTAINTY_ASSIGNED_CONTEXT((#12346))
GLOBAL_UNIT_ASSIGNED_CONTEXT((#12414,#12416,#12417))
REPRESENTATION_CONTEXT('','3D')
);
#12393=(
GEOMETRIC_REPRESENTATION_CONTEXT(3)
GLOBAL_UNCERTAINTY_ASSIGNED_CONTEXT((#12347))
GLOBAL_UNIT_ASSIGNED_CONTEXT((#12414,#12416,#12417))
REPRESENTATION_CONTEXT('','3D')
);
#12394=(
GEOMETRIC_REPRESENTATION_CONTEXT(3)
GLOBAL_UNCERTAINTY_ASSIGNED_CONTEXT((#12348))
GLOBAL_UNIT_ASSIGNED_CONTEXT((#12414,#12416,#12417))
REPRESENTATION_CONTEXT('','3D')
);
#12395=(
GEOMETRIC_REPRESENTATION_CONTEXT(3)
GLOBAL_UNCERTAINTY_ASSIGNED_CONTEXT((#12349))
GLOBAL_UNIT_ASSIGNED_CONTEXT((#12414,#12416,#12417))
REPRESENTATION_CONTEXT('','3D')
);
#12396=(
GEOMETRIC_REPRESENTATION_CONTEXT(3)
GLOBAL_UNCERTAINTY_ASSIGNED_CONTEXT((#12350))
GLOBAL_UNIT_ASSIGNED_CONTEXT((#12414,#12416,#12417))
REPRESENTATION_CONTEXT('','3D')
);
#12397=(
GEOMETRIC_REPRESENTATION_CONTEXT(3)
GLOBAL_UNCERTAINTY_ASSIGNED_CONTEXT((#12351))
GLOBAL_UNIT_ASSIGNED_CONTEXT((#12414,#12416,#12417))
REPRESENTATION_CONTEXT('','3D')
);
#12398=(
GEOMETRIC_REPRESENTATION_CONTEXT(3)
GLOBAL_UNCERTAINTY_ASSIGNED_CONTEXT((#12352))
GLOBAL_UNIT_ASSIGNED_CONTEXT((#12414,#12416,#12417))
REPRESENTATION_CONTEXT('','3D')
);
#12399=(
GEOMETRIC_REPRESENTATION_CONTEXT(3)
GLOBAL_UNCERTAINTY_ASSIGNED_CONTEXT((#12353))
GLOBAL_UNIT_ASSIGNED_CONTEXT((#12414,#12416,#12417))
REPRESENTATION_CONTEXT('','3D')
);
#12400=(
GEOMETRIC_REPRESENTATION_CONTEXT(3)
GLOBAL_UNCERTAINTY_ASSIGNED_CONTEXT((#12354))
GLOBAL_UNIT_ASSIGNED_CONTEXT((#12414,#12416,#12417))
REPRESENTATION_CONTEXT('','3D')
);
#12401=(
GEOMETRIC_REPRESENTATION_CONTEXT(3)
GLOBAL_UNCERTAINTY_ASSIGNED_CONTEXT((#12355))
GLOBAL_UNIT_ASSIGNED_CONTEXT((#12414,#12416,#12417))
REPRESENTATION_CONTEXT('','3D')
);
#12402=(
GEOMETRIC_REPRESENTATION_CONTEXT(3)
GLOBAL_UNCERTAINTY_ASSIGNED_CONTEXT((#12356))
GLOBAL_UNIT_ASSIGNED_CONTEXT((#12414,#12416,#12417))
REPRESENTATION_CONTEXT('','3D')
);
#12403=(
GEOMETRIC_REPRESENTATION_CONTEXT(3)
GLOBAL_UNCERTAINTY_ASSIGNED_CONTEXT((#12357))
GLOBAL_UNIT_ASSIGNED_CONTEXT((#12414,#12416,#12417))
REPRESENTATION_CONTEXT('','3D')
);
#12404=(
GEOMETRIC_REPRESENTATION_CONTEXT(3)
GLOBAL_UNCERTAINTY_ASSIGNED_CONTEXT((#12358))
GLOBAL_UNIT_ASSIGNED_CONTEXT((#12414,#12416,#12417))
REPRESENTATION_CONTEXT('','3D')
);
#12405=(
GEOMETRIC_REPRESENTATION_CONTEXT(3)
GLOBAL_UNCERTAINTY_ASSIGNED_CONTEXT((#12359))
GLOBAL_UNIT_ASSIGNED_CONTEXT((#12414,#12416,#12417))
REPRESENTATION_CONTEXT('','3D')
);
#12406=(
GEOMETRIC_REPRESENTATION_CONTEXT(3)
GLOBAL_UNCERTAINTY_ASSIGNED_CONTEXT((#12360))
GLOBAL_UNIT_ASSIGNED_CONTEXT((#12414,#12416,#12417))
REPRESENTATION_CONTEXT('','3D')
);
#12407=(
GEOMETRIC_REPRESENTATION_CONTEXT(3)
GLOBAL_UNCERTAINTY_ASSIGNED_CONTEXT((#12361))
GLOBAL_UNIT_ASSIGNED_CONTEXT((#12414,#12416,#12417))
REPRESENTATION_CONTEXT('','3D')
);
#12408=(
GEOMETRIC_REPRESENTATION_CONTEXT(3)
GLOBAL_UNCERTAINTY_ASSIGNED_CONTEXT((#12362))
GLOBAL_UNIT_ASSIGNED_CONTEXT((#12414,#12416,#12417))
REPRESENTATION_CONTEXT('','3D')
);
#12409=(
GEOMETRIC_REPRESENTATION_CONTEXT(3)
GLOBAL_UNCERTAINTY_ASSIGNED_CONTEXT((#12363))
GLOBAL_UNIT_ASSIGNED_CONTEXT((#12414,#12416,#12417))
REPRESENTATION_CONTEXT('','3D')
);
#12410=(
GEOMETRIC_REPRESENTATION_CONTEXT(3)
GLOBAL_UNCERTAINTY_ASSIGNED_CONTEXT((#12364))
GLOBAL_UNIT_ASSIGNED_CONTEXT((#12414,#12416,#12417))
REPRESENTATION_CONTEXT('','3D')
);
#12411=(
GEOMETRIC_REPRESENTATION_CONTEXT(3)
GLOBAL_UNCERTAINTY_ASSIGNED_CONTEXT((#12365))
GLOBAL_UNIT_ASSIGNED_CONTEXT((#12414,#12416,#12417))
REPRESENTATION_CONTEXT('','3D')
);
#12412=(
GEOMETRIC_REPRESENTATION_CONTEXT(3)
GLOBAL_UNCERTAINTY_ASSIGNED_CONTEXT((#12366))
GLOBAL_UNIT_ASSIGNED_CONTEXT((#12414,#12416,#12417))
REPRESENTATION_CONTEXT('','3D')
);
#12413=(
GEOMETRIC_REPRESENTATION_CONTEXT(3)
GLOBAL_UNCERTAINTY_ASSIGNED_CONTEXT((#12367))
GLOBAL_UNIT_ASSIGNED_CONTEXT((#12414,#12416,#12417))
REPRESENTATION_CONTEXT('','3D')
);
#12414=(
LENGTH_UNIT()
NAMED_UNIT(*)
SI_UNIT(.CENTI.,.METRE.)
);
#12415=(
LENGTH_UNIT()
NAMED_UNIT(*)
SI_UNIT($,.METRE.)
);
#12416=(
NAMED_UNIT(*)
PLANE_ANGLE_UNIT()
SI_UNIT($,.RADIAN.)
);
#12417=(
NAMED_UNIT(*)
SI_UNIT($,.STERADIAN.)
SOLID_ANGLE_UNIT()
);
#12418=SHAPE_DEFINITION_REPRESENTATION(#12463,#12571);
#12419=SHAPE_DEFINITION_REPRESENTATION(#12464,#12572);
#12420=SHAPE_DEFINITION_REPRESENTATION(#12465,#12573);
#12421=SHAPE_DEFINITION_REPRESENTATION(#12466,#12574);
#12422=SHAPE_DEFINITION_REPRESENTATION(#12467,#12575);
#12423=SHAPE_DEFINITION_REPRESENTATION(#12468,#12576);
#12424=SHAPE_DEFINITION_REPRESENTATION(#12469,#12577);
#12425=SHAPE_DEFINITION_REPRESENTATION(#12470,#12578);
#12426=SHAPE_DEFINITION_REPRESENTATION(#12471,#12579);
#12427=SHAPE_DEFINITION_REPRESENTATION(#12472,#12580);
#12428=SHAPE_DEFINITION_REPRESENTATION(#12473,#12581);
#12429=SHAPE_DEFINITION_REPRESENTATION(#12474,#12582);
#12430=SHAPE_DEFINITION_REPRESENTATION(#12475,#12583);
#12431=SHAPE_DEFINITION_REPRESENTATION(#12476,#12584);
#12432=SHAPE_DEFINITION_REPRESENTATION(#12477,#12585);
#12433=SHAPE_DEFINITION_REPRESENTATION(#12478,#12586);
#12434=SHAPE_DEFINITION_REPRESENTATION(#12479,#12587);
#12435=SHAPE_DEFINITION_REPRESENTATION(#12480,#12588);
#12436=SHAPE_DEFINITION_REPRESENTATION(#12481,#12589);
#12437=SHAPE_DEFINITION_REPRESENTATION(#12482,#12590);
#12438=SHAPE_DEFINITION_REPRESENTATION(#12488,#12591);
#12439=SHAPE_DEFINITION_REPRESENTATION(#12489,#12592);
#12440=SHAPE_DEFINITION_REPRESENTATION(#12490,#12593);
#12441=SHAPE_DEFINITION_REPRESENTATION(#12493,#12594);
#12442=SHAPE_DEFINITION_REPRESENTATION(#12494,#12595);
#12443=SHAPE_DEFINITION_REPRESENTATION(#12495,#12596);
#12444=SHAPE_DEFINITION_REPRESENTATION(#12496,#12597);
#12445=SHAPE_DEFINITION_REPRESENTATION(#12497,#12598);
#12446=SHAPE_DEFINITION_REPRESENTATION(#12498,#12599);
#12447=SHAPE_DEFINITION_REPRESENTATION(#12499,#12600);
#12448=SHAPE_DEFINITION_REPRESENTATION(#12500,#12601);
#12449=SHAPE_DEFINITION_REPRESENTATION(#12501,#12602);
#12450=SHAPE_DEFINITION_REPRESENTATION(#12502,#12603);
#12451=SHAPE_DEFINITION_REPRESENTATION(#12503,#12604);
#12452=SHAPE_DEFINITION_REPRESENTATION(#12504,#12605);
#12453=SHAPE_DEFINITION_REPRESENTATION(#12505,#12606);
#12454=SHAPE_DEFINITION_REPRESENTATION(#12551,#12607);
#12455=SHAPE_DEFINITION_REPRESENTATION(#12552,#12608);
#12456=SHAPE_DEFINITION_REPRESENTATION(#12553,#12609);
#12457=SHAPE_DEFINITION_REPRESENTATION(#12554,#12610);
#12458=SHAPE_DEFINITION_REPRESENTATION(#12558,#12611);
#12459=SHAPE_DEFINITION_REPRESENTATION(#12559,#12612);
#12460=SHAPE_DEFINITION_REPRESENTATION(#12560,#12613);
#12461=SHAPE_DEFINITION_REPRESENTATION(#12561,#12614);
#12462=SHAPE_DEFINITION_REPRESENTATION(#12562,#12615);
#12463=PRODUCT_DEFINITION_SHAPE('',$,#12617);
#12464=PRODUCT_DEFINITION_SHAPE('',$,#12618);
#12465=PRODUCT_DEFINITION_SHAPE('',$,#12619);
#12466=PRODUCT_DEFINITION_SHAPE('',$,#12620);
#12467=PRODUCT_DEFINITION_SHAPE('',$,#12621);
#12468=PRODUCT_DEFINITION_SHAPE('',$,#12622);
#12469=PRODUCT_DEFINITION_SHAPE('',$,#12623);
#12470=PRODUCT_DEFINITION_SHAPE('',$,#12624);
#12471=PRODUCT_DEFINITION_SHAPE('',$,#12625);
#12472=PRODUCT_DEFINITION_SHAPE('',$,#12626);
#12473=PRODUCT_DEFINITION_SHAPE('',$,#12627);
#12474=PRODUCT_DEFINITION_SHAPE('',$,#12628);
#12475=PRODUCT_DEFINITION_SHAPE('',$,#12629);
#12476=PRODUCT_DEFINITION_SHAPE('',$,#12630);
#12477=PRODUCT_DEFINITION_SHAPE('',$,#12631);
#12478=PRODUCT_DEFINITION_SHAPE('',$,#12632);
#12479=PRODUCT_DEFINITION_SHAPE('',$,#12633);
#12480=PRODUCT_DEFINITION_SHAPE('',$,#12634);
#12481=PRODUCT_DEFINITION_SHAPE('',$,#12635);
#12482=PRODUCT_DEFINITION_SHAPE('',$,#12636);
#12483=PRODUCT_DEFINITION_SHAPE($,$,#200);
#12484=PRODUCT_DEFINITION_SHAPE($,$,#201);
#12485=PRODUCT_DEFINITION_SHAPE($,$,#202);
#12486=PRODUCT_DEFINITION_SHAPE($,$,#203);
#12487=PRODUCT_DEFINITION_SHAPE($,$,#204);
#12488=PRODUCT_DEFINITION_SHAPE('',$,#12637);
#12489=PRODUCT_DEFINITION_SHAPE('',$,#12638);
#12490=PRODUCT_DEFINITION_SHAPE('',$,#12639);
#12491=PRODUCT_DEFINITION_SHAPE($,$,#205);
#12492=PRODUCT_DEFINITION_SHAPE($,$,#206);
#12493=PRODUCT_DEFINITION_SHAPE('',$,#12640);
#12494=PRODUCT_DEFINITION_SHAPE('',$,#12641);
#12495=PRODUCT_DEFINITION_SHAPE('',$,#12642);
#12496=PRODUCT_DEFINITION_SHAPE('',$,#12643);
#12497=PRODUCT_DEFINITION_SHAPE('',$,#12644);
#12498=PRODUCT_DEFINITION_SHAPE('',$,#12645);
#12499=PRODUCT_DEFINITION_SHAPE('',$,#12646);
#12500=PRODUCT_DEFINITION_SHAPE('',$,#12647);
#12501=PRODUCT_DEFINITION_SHAPE('',$,#12648);
#12502=PRODUCT_DEFINITION_SHAPE('',$,#12649);
#12503=PRODUCT_DEFINITION_SHAPE('',$,#12650);
#12504=PRODUCT_DEFINITION_SHAPE('',$,#12651);
#12505=PRODUCT_DEFINITION_SHAPE('',$,#12652);
#12506=PRODUCT_DEFINITION_SHAPE($,$,#207);
#12507=PRODUCT_DEFINITION_SHAPE($,$,#208);
#12508=PRODUCT_DEFINITION_SHAPE($,$,#209);
#12509=PRODUCT_DEFINITION_SHAPE($,$,#210);
#12510=PRODUCT_DEFINITION_SHAPE($,$,#211);
#12511=PRODUCT_DEFINITION_SHAPE($,$,#212);
#12512=PRODUCT_DEFINITION_SHAPE($,$,#213);
#12513=PRODUCT_DEFINITION_SHAPE($,$,#214);
#12514=PRODUCT_DEFINITION_SHAPE($,$,#215);
#12515=PRODUCT_DEFINITION_SHAPE($,$,#216);
#12516=PRODUCT_DEFINITION_SHAPE($,$,#217);
#12517=PRODUCT_DEFINITION_SHAPE($,$,#218);
#12518=PRODUCT_DEFINITION_SHAPE($,$,#219);
#12519=PRODUCT_DEFINITION_SHAPE($,$,#220);
#12520=PRODUCT_DEFINITION_SHAPE($,$,#221);
#12521=PRODUCT_DEFINITION_SHAPE($,$,#222);
#12522=PRODUCT_DEFINITION_SHAPE($,$,#223);
#12523=PRODUCT_DEFINITION_SHAPE($,$,#224);
#12524=PRODUCT_DEFINITION_SHAPE($,$,#225);
#12525=PRODUCT_DEFINITION_SHAPE($,$,#226);
#12526=PRODUCT_DEFINITION_SHAPE($,$,#227);
#12527=PRODUCT_DEFINITION_SHAPE($,$,#228);
#12528=PRODUCT_DEFINITION_SHAPE($,$,#229);
#12529=PRODUCT_DEFINITION_SHAPE($,$,#230);
#12530=PRODUCT_DEFINITION_SHAPE($,$,#231);
#12531=PRODUCT_DEFINITION_SHAPE($,$,#232);
#12532=PRODUCT_DEFINITION_SHAPE($,$,#233);
#12533=PRODUCT_DEFINITION_SHAPE($,$,#234);
#12534=PRODUCT_DEFINITION_SHAPE($,$,#235);
#12535=PRODUCT_DEFINITION_SHAPE($,$,#236);
#12536=PRODUCT_DEFINITION_SHAPE($,$,#237);
#12537=PRODUCT_DEFINITION_SHAPE($,$,#238);
#12538=PRODUCT_DEFINITION_SHAPE($,$,#239);
#12539=PRODUCT_DEFINITION_SHAPE($,$,#240);
#12540=PRODUCT_DEFINITION_SHAPE($,$,#241);
#12541=PRODUCT_DEFINITION_SHAPE($,$,#242);
#12542=PRODUCT_DEFINITION_SHAPE($,$,#243);
#12543=PRODUCT_DEFINITION_SHAPE($,$,#244);
#12544=PRODUCT_DEFINITION_SHAPE($,$,#245);
#12545=PRODUCT_DEFINITION_SHAPE($,$,#246);
#12546=PRODUCT_DEFINITION_SHAPE($,$,#247);
#12547=PRODUCT_DEFINITION_SHAPE($,$,#248);
#12548=PRODUCT_DEFINITION_SHAPE($,$,#249);
#12549=PRODUCT_DEFINITION_SHAPE($,$,#250);
#12550=PRODUCT_DEFINITION_SHAPE($,$,#251);
#12551=PRODUCT_DEFINITION_SHAPE('',$,#12653);
#12552=PRODUCT_DEFINITION_SHAPE('',$,#12654);
#12553=PRODUCT_DEFINITION_SHAPE('',$,#12655);
#12554=PRODUCT_DEFINITION_SHAPE('',$,#12656);
#12555=PRODUCT_DEFINITION_SHAPE($,$,#252);
#12556=PRODUCT_DEFINITION_SHAPE($,$,#253);
#12557=PRODUCT_DEFINITION_SHAPE($,$,#254);
#12558=PRODUCT_DEFINITION_SHAPE('',$,#12657);
#12559=PRODUCT_DEFINITION_SHAPE('',$,#12658);
#12560=PRODUCT_DEFINITION_SHAPE('',$,#12659);
#12561=PRODUCT_DEFINITION_SHAPE('',$,#12660);
#12562=PRODUCT_DEFINITION_SHAPE('',$,#12661);
#12563=PRODUCT_DEFINITION_SHAPE($,$,#255);
#12564=PRODUCT_DEFINITION_SHAPE($,$,#256);
#12565=PRODUCT_DEFINITION_SHAPE($,$,#257);
#12566=PRODUCT_DEFINITION_SHAPE($,$,#258);
#12567=PRODUCT_DEFINITION_SHAPE($,$,#259);
#12568=PRODUCT_DEFINITION_SHAPE($,$,#260);
#12569=PRODUCT_DEFINITION_SHAPE($,$,#261);
#12570=PRODUCT_DEFINITION_SHAPE($,$,#262);
#12571=SHAPE_REPRESENTATION('',(#7039,#7890,#7891,#7892,#7893),#12368);
#12572=SHAPE_REPRESENTATION('',(#7040,#7728,#7729,#7730,#7731,#7732,#7733,
#7734,#7735,#7736,#7737,#7738,#7739,#7740,#7741,#7742,#7743,#7744,#7745,
#7746,#7747,#7748,#7749,#7750,#7751,#7752,#7753,#7754,#7755,#7756,#7757,
#7758,#7759,#7760,#7761),#12369);
#12573=SHAPE_REPRESENTATION('',(#7041),#12370);
#12574=SHAPE_REPRESENTATION('',(#7072),#12371);
#12575=SHAPE_REPRESENTATION('',(#7079),#12372);
#12576=SHAPE_REPRESENTATION('',(#7086),#12373);
#12577=SHAPE_REPRESENTATION('',(#7161),#12374);
#12578=SHAPE_REPRESENTATION('',(#7186),#12375);
#12579=SHAPE_REPRESENTATION('',(#7211),#12376);
#12580=SHAPE_REPRESENTATION('',(#7252),#12377);
#12581=SHAPE_REPRESENTATION('',(#7259),#12378);
#12582=SHAPE_REPRESENTATION('',(#7274),#12379);
#12583=SHAPE_REPRESENTATION('',(#7289),#12380);
#12584=SHAPE_REPRESENTATION('',(#7303),#12381);
#12585=SHAPE_REPRESENTATION('',(#7327,#7456,#7457,#7458,#7459,#7460),#12382);
#12586=SHAPE_REPRESENTATION('',(#7328),#12383);
#12587=SHAPE_REPRESENTATION('',(#7348),#12384);
#12588=SHAPE_REPRESENTATION('',(#7368),#12385);
#12589=SHAPE_REPRESENTATION('',(#7385),#12386);
#12590=SHAPE_REPRESENTATION('',(#7439),#12387);
#12591=SHAPE_REPRESENTATION('',(#7461,#7511,#7512),#12388);
#12592=SHAPE_REPRESENTATION('',(#7462),#12389);
#12593=SHAPE_REPRESENTATION('',(#7494),#12390);
#12594=SHAPE_REPRESENTATION('',(#7513),#12391);
#12595=SHAPE_REPRESENTATION('',(#7543,#7762,#7763,#7764,#7765,#7766,#7767,
#7768,#7769,#7770,#7771,#7772),#12392);
#12596=SHAPE_REPRESENTATION('',(#7544),#12393);
#12597=SHAPE_REPRESENTATION('',(#7581),#12394);
#12598=SHAPE_REPRESENTATION('',(#7590),#12395);
#12599=SHAPE_REPRESENTATION('',(#7605),#12396);
#12600=SHAPE_REPRESENTATION('',(#7627),#12397);
#12601=SHAPE_REPRESENTATION('',(#7636),#12398);
#12602=SHAPE_REPRESENTATION('',(#7645),#12399);
#12603=SHAPE_REPRESENTATION('',(#7654),#12400);
#12604=SHAPE_REPRESENTATION('',(#7663),#12401);
#12605=SHAPE_REPRESENTATION('',(#7678),#12402);
#12606=SHAPE_REPRESENTATION('',(#7702),#12403);
#12607=SHAPE_REPRESENTATION('',(#7773,#7809,#7810,#7811),#12404);
#12608=SHAPE_REPRESENTATION('',(#7774),#12405);
#12609=SHAPE_REPRESENTATION('',(#7791),#12406);
#12610=SHAPE_REPRESENTATION('',(#7800),#12407);
#12611=SHAPE_REPRESENTATION('',(#7812,#7886,#7887,#7888,#7889),#12408);
#12612=SHAPE_REPRESENTATION('',(#7813),#12409);
#12613=SHAPE_REPRESENTATION('',(#7853),#12410);
#12614=SHAPE_REPRESENTATION('',(#7863),#12411);
#12615=SHAPE_REPRESENTATION('',(#7869),#12412);
#12616=PRODUCT_DEFINITION_CONTEXT('part definition',#12753,'design');
#12617=PRODUCT_DEFINITION('PAT-066',
'PAT-066',#12662,#12616);
#12618=PRODUCT_DEFINITION('Base and guide','Base and guide',#12663,#12616);
#12619=PRODUCT_DEFINITION('Base','Base',#12664,#12616);
#12620=PRODUCT_DEFINITION('Foot strip','Foot strip',#12665,#12616);
#12621=PRODUCT_DEFINITION('Foot strip (1)','Foot strip (1)',#12666,#12616);
#12622=PRODUCT_DEFINITION('Bearing frame','Bearing frame',#12667,#12616);
#12623=PRODUCT_DEFINITION('Front bearing cap','Front bearing cap',#12668,
#12616);
#12624=PRODUCT_DEFINITION('Rear bearing cap','Rear bearing cap',#12669,
#12616);
#12625=PRODUCT_DEFINITION('Linear bearing cap','Linear bearing cap',#12670,
#12616);
#12626=PRODUCT_DEFINITION('Bar specimen envelope',
'Bar specimen envelope',#12671,#12616);
#12627=PRODUCT_DEFINITION('Left bar guide','Left bar guide',#12672,#12616);
#12628=PRODUCT_DEFINITION('Right bar guide','Right bar guide',#12673,#12616);
#12629=PRODUCT_DEFINITION('Closed lever stop','Closed lever stop',#12674,
#12616);
#12630=PRODUCT_DEFINITION('M5x14 Cap Screw','M5x14 Cap Screw',#12675,#12616);
#12631=PRODUCT_DEFINITION('Sealed Ball Bearing - 10 x 30 x 9 mm',
'Sealed Ball Bearing - 10 x 30 x 9 mm',#12676,#12616);
#12632=PRODUCT_DEFINITION('Inner ring','Inner ring',#12677,#12616);
#12633=PRODUCT_DEFINITION('Outer ring','Outer ring',#12678,#12616);
#12634=PRODUCT_DEFINITION('Balls','Balls',#12679,#12616);
#12635=PRODUCT_DEFINITION('Cage','Cage',#12680,#12616);
#12636=PRODUCT_DEFINITION('Seals 2RS','Seals 2RS',#12681,#12616);
#12637=PRODUCT_DEFINITION('Linear Ball Bushing - 12 x 21 x 30 mm',
'Linear Ball Bushing - 12 x 21 x 30 mm',#12682,#12616);
#12638=PRODUCT_DEFINITION('Steel sleeve','Steel sleeve',#12683,#12616);
#12639=PRODUCT_DEFINITION('Ball retainer (plastic)',
'Ball retainer (plastic)',#12684,#12616);
#12640=PRODUCT_DEFINITION('M4x30 stop screw','M4x30 stop screw',#12685,
#12616);
#12641=PRODUCT_DEFINITION('Operating lever','Operating lever',#12686,#12616);
#12642=PRODUCT_DEFINITION('Lever and spindle','Lever and spindle',#12687,
#12616);
#12643=PRODUCT_DEFINITION('Inner race spacer','Inner race spacer',#12688,
#12616);
#12644=PRODUCT_DEFINITION('Shaft collar','Shaft collar',#12689,#12616);
#12645=PRODUCT_DEFINITION('Lever link pin','Lever link pin',#12690,#12616);
#12646=PRODUCT_DEFINITION('Rear pin spacer','Rear pin spacer',#12691,#12616);
#12647=PRODUCT_DEFINITION('Front pin spacer','Front pin spacer',#12692,
#12616);
#12648=PRODUCT_DEFINITION('Front pin keeper','Front pin keeper',#12693,
#12616);
#12649=PRODUCT_DEFINITION('Rear pin keeper','Rear pin keeper',#12694,#12616);
#12650=PRODUCT_DEFINITION('M4x4 collar screw','M4x4 collar screw',#12695,
#12616);
#12651=PRODUCT_DEFINITION('M4x10 Cap Screw','M4x10 Cap Screw',#12696,#12616);
#12652=PRODUCT_DEFINITION('Cap Screw - M4x16','Cap Screw - M4x16',#12697,
#12616);
#12653=PRODUCT_DEFINITION('Connecting link (1)','Connecting link (1)',#12698,
#12616);
#12654=PRODUCT_DEFINITION('Connecting link','Connecting link',#12699,
#12616);
#12655=PRODUCT_DEFINITION('Link bush','Link bush',#12700,#12616);
#12656=PRODUCT_DEFINITION('Link bush (1)','Link bush (1)',#12701,#12616);
#12657=PRODUCT_DEFINITION('Pressure plunger','Pressure plunger',#12702,
#12616);
#12658=PRODUCT_DEFINITION('Plunger and fork','Plunger and fork',#12703,
#12616);
#12659=PRODUCT_DEFINITION('Fork pin','Fork pin',#12704,#12616);
#12660=PRODUCT_DEFINITION('Elastomer pressure pad installed',
'Elastomer pressure pad installed',#12705,#12616);
#12661=PRODUCT_DEFINITION('Socket Set Screw - M4x6',
'Socket Set Screw - M4x6',#12706,#12616);
#12662=PRODUCT_DEFINITION_FORMATION('',$,#12755);
#12663=PRODUCT_DEFINITION_FORMATION('',$,#12756);
#12664=PRODUCT_DEFINITION_FORMATION('',$,#12757);
#12665=PRODUCT_DEFINITION_FORMATION('',$,#12758);
#12666=PRODUCT_DEFINITION_FORMATION('',$,#12759);
#12667=PRODUCT_DEFINITION_FORMATION('',$,#12760);
#12668=PRODUCT_DEFINITION_FORMATION('',$,#12761);
#12669=PRODUCT_DEFINITION_FORMATION('',$,#12762);
#12670=PRODUCT_DEFINITION_FORMATION('',$,#12763);
#12671=PRODUCT_DEFINITION_FORMATION('',$,#12764);
#12672=PRODUCT_DEFINITION_FORMATION('',$,#12765);
#12673=PRODUCT_DEFINITION_FORMATION('',$,#12766);
#12674=PRODUCT_DEFINITION_FORMATION('',$,#12767);
#12675=PRODUCT_DEFINITION_FORMATION('',$,#12768);
#12676=PRODUCT_DEFINITION_FORMATION('',$,#12769);
#12677=PRODUCT_DEFINITION_FORMATION('',$,#12770);
#12678=PRODUCT_DEFINITION_FORMATION('',$,#12771);
#12679=PRODUCT_DEFINITION_FORMATION('',$,#12772);
#12680=PRODUCT_DEFINITION_FORMATION('',$,#12773);
#12681=PRODUCT_DEFINITION_FORMATION('',$,#12774);
#12682=PRODUCT_DEFINITION_FORMATION('',$,#12775);
#12683=PRODUCT_DEFINITION_FORMATION('',$,#12776);
#12684=PRODUCT_DEFINITION_FORMATION('',$,#12777);
#12685=PRODUCT_DEFINITION_FORMATION('',$,#12778);
#12686=PRODUCT_DEFINITION_FORMATION('',$,#12779);
#12687=PRODUCT_DEFINITION_FORMATION('',$,#12780);
#12688=PRODUCT_DEFINITION_FORMATION('',$,#12781);
#12689=PRODUCT_DEFINITION_FORMATION('',$,#12782);
#12690=PRODUCT_DEFINITION_FORMATION('',$,#12783);
#12691=PRODUCT_DEFINITION_FORMATION('',$,#12784);
#12692=PRODUCT_DEFINITION_FORMATION('',$,#12785);
#12693=PRODUCT_DEFINITION_FORMATION('',$,#12786);
#12694=PRODUCT_DEFINITION_FORMATION('',$,#12787);
#12695=PRODUCT_DEFINITION_FORMATION('',$,#12788);
#12696=PRODUCT_DEFINITION_FORMATION('',$,#12789);
#12697=PRODUCT_DEFINITION_FORMATION('',$,#12790);
#12698=PRODUCT_DEFINITION_FORMATION('',$,#12791);
#12699=PRODUCT_DEFINITION_FORMATION('',$,#12792);
#12700=PRODUCT_DEFINITION_FORMATION('',$,#12793);
#12701=PRODUCT_DEFINITION_FORMATION('',$,#12794);
#12702=PRODUCT_DEFINITION_FORMATION('',$,#12795);
#12703=PRODUCT_DEFINITION_FORMATION('',$,#12796);
#12704=PRODUCT_DEFINITION_FORMATION('',$,#12797);
#12705=PRODUCT_DEFINITION_FORMATION('',$,#12798);
#12706=PRODUCT_DEFINITION_FORMATION('',$,#12799);
#12707=PRODUCT_RELATED_PRODUCT_CATEGORY('PAT-066','PAT-066',(#12755));
#12708=PRODUCT_RELATED_PRODUCT_CATEGORY('Base and guide',
'Base and guide',(#12756));
#12709=PRODUCT_RELATED_PRODUCT_CATEGORY('Base','Base',(#12757));
#12710=PRODUCT_RELATED_PRODUCT_CATEGORY('Foot strip','Foot strip',(#12758));
#12711=PRODUCT_RELATED_PRODUCT_CATEGORY('Foot strip (1)',
'Foot strip (1)',(#12759));
#12712=PRODUCT_RELATED_PRODUCT_CATEGORY('Bearing frame','Bearing frame',
(#12760));
#12713=PRODUCT_RELATED_PRODUCT_CATEGORY('Front bearing cap',
'Front bearing cap',(#12761));
#12714=PRODUCT_RELATED_PRODUCT_CATEGORY('Rear bearing cap',
'Rear bearing cap',(#12762));
#12715=PRODUCT_RELATED_PRODUCT_CATEGORY('Linear bearing cap',
'Linear bearing cap',(#12763));
#12716=PRODUCT_RELATED_PRODUCT_CATEGORY('Bar specimen envelope',
'Bar specimen envelope',(#12764));
#12717=PRODUCT_RELATED_PRODUCT_CATEGORY('Left bar guide',
'Left bar guide',(#12765));
#12718=PRODUCT_RELATED_PRODUCT_CATEGORY('Right bar guide',
'Right bar guide',(#12766));
#12719=PRODUCT_RELATED_PRODUCT_CATEGORY('Closed lever stop',
'Closed lever stop',(#12767));
#12720=PRODUCT_RELATED_PRODUCT_CATEGORY('M5x14 Cap Screw',
'M5x14 Cap Screw',(#12768));
#12721=PRODUCT_RELATED_PRODUCT_CATEGORY(
'Sealed Ball Bearing - 10 x 30 x 9 mm',
'Sealed Ball Bearing - 10 x 30 x 9 mm',(#12769));
#12722=PRODUCT_RELATED_PRODUCT_CATEGORY('Inner ring','Inner ring',(#12770));
#12723=PRODUCT_RELATED_PRODUCT_CATEGORY('Outer ring','Outer ring',(#12771));
#12724=PRODUCT_RELATED_PRODUCT_CATEGORY('Balls','Balls',(#12772));
#12725=PRODUCT_RELATED_PRODUCT_CATEGORY('Cage','Cage',(#12773));
#12726=PRODUCT_RELATED_PRODUCT_CATEGORY('Seals 2RS','Seals 2RS',(#12774));
#12727=PRODUCT_RELATED_PRODUCT_CATEGORY(
'Linear Ball Bushing - 12 x 21 x 30 mm',
'Linear Ball Bushing - 12 x 21 x 30 mm',(#12775));
#12728=PRODUCT_RELATED_PRODUCT_CATEGORY('Steel sleeve','Steel sleeve',(#12776));
#12729=PRODUCT_RELATED_PRODUCT_CATEGORY('Ball retainer (plastic)',
'Ball retainer (plastic)',(#12777));
#12730=PRODUCT_RELATED_PRODUCT_CATEGORY('M4x30 stop screw',
'M4x30 stop screw',(#12778));
#12731=PRODUCT_RELATED_PRODUCT_CATEGORY('Operating lever',
'Operating lever',(#12779));
#12732=PRODUCT_RELATED_PRODUCT_CATEGORY('Lever and spindle',
'Lever and spindle',(#12780));
#12733=PRODUCT_RELATED_PRODUCT_CATEGORY('Inner race spacer',
'Inner race spacer',(#12781));
#12734=PRODUCT_RELATED_PRODUCT_CATEGORY('Shaft collar','Shaft collar',(#12782));
#12735=PRODUCT_RELATED_PRODUCT_CATEGORY('Lever link pin',
'Lever link pin',(#12783));
#12736=PRODUCT_RELATED_PRODUCT_CATEGORY('Rear pin spacer',
'Rear pin spacer',(#12784));
#12737=PRODUCT_RELATED_PRODUCT_CATEGORY('Front pin spacer',
'Front pin spacer',(#12785));
#12738=PRODUCT_RELATED_PRODUCT_CATEGORY('Front pin keeper',
'Front pin keeper',(#12786));
#12739=PRODUCT_RELATED_PRODUCT_CATEGORY('Rear pin keeper',
'Rear pin keeper',(#12787));
#12740=PRODUCT_RELATED_PRODUCT_CATEGORY('M4x4 collar screw',
'M4x4 collar screw',(#12788));
#12741=PRODUCT_RELATED_PRODUCT_CATEGORY('M4x10 Cap Screw',
'M4x10 Cap Screw',(#12789));
#12742=PRODUCT_RELATED_PRODUCT_CATEGORY('Cap Screw - M4x16',
'Cap Screw - M4x16',(#12790));
#12743=PRODUCT_RELATED_PRODUCT_CATEGORY('Connecting link (1)',
'Connecting link (1)',(#12791));
#12744=PRODUCT_RELATED_PRODUCT_CATEGORY('Connecting link',
'Connecting link',(#12792));
#12745=PRODUCT_RELATED_PRODUCT_CATEGORY('Link bush','Link bush',(#12793));
#12746=PRODUCT_RELATED_PRODUCT_CATEGORY('Link bush (1)','Link bush (1)',
(#12794));
#12747=PRODUCT_RELATED_PRODUCT_CATEGORY('Pressure plunger',
'Pressure plunger',(#12795));
#12748=PRODUCT_RELATED_PRODUCT_CATEGORY('Plunger and fork',
'Plunger and fork',(#12796));
#12749=PRODUCT_RELATED_PRODUCT_CATEGORY('Fork pin','Fork pin',(#12797));
#12750=PRODUCT_RELATED_PRODUCT_CATEGORY(
'Elastomer pressure pad installed','Elastomer pressure pad installed',(#12798));
#12751=PRODUCT_RELATED_PRODUCT_CATEGORY('Socket Set Screw - M4x6',
'Socket Set Screw - M4x6',(#12799));
#12752=APPLICATION_PROTOCOL_DEFINITION('international standard',
'automotive_design',2009,#12753);
#12753=APPLICATION_CONTEXT(
'Core Data for Automotive Mechanical Design Process');
#12754=PRODUCT_CONTEXT('part definition',#12753,'mechanical');
#12755=PRODUCT('PAT-066','PAT-066',
'PAT-066',(#12754));
#12756=PRODUCT('Base and guide','Base and guide','Base and guide',(#12754));
#12757=PRODUCT('Base','Base','Base',(#12754));
#12758=PRODUCT('Foot strip','Foot strip','Foot strip',(#12754));
#12759=PRODUCT('Foot strip (1)','Foot strip (1)','Foot strip (1)',(#12754));
#12760=PRODUCT('Bearing frame','Bearing frame','Bearing frame',(#12754));
#12761=PRODUCT('Front bearing cap','Front bearing cap',
'Front bearing cap',(#12754));
#12762=PRODUCT('Rear bearing cap','Rear bearing cap','Rear bearing cap',
(#12754));
#12763=PRODUCT('Linear bearing cap','Linear bearing cap',
'Linear bearing cap',(#12754));
#12764=PRODUCT('Bar specimen envelope','Bar specimen envelope',
'Bar specimen envelope',(#12754));
#12765=PRODUCT('Left bar guide','Left bar guide','Left bar guide',(#12754));
#12766=PRODUCT('Right bar guide','Right bar guide','Right bar guide',(#12754));
#12767=PRODUCT('Closed lever stop','Closed lever stop',
'Closed lever stop',(#12754));
#12768=PRODUCT('M5x14 Cap Screw','M5x14 Cap Screw','M5x14 Cap Screw',(#12754));
#12769=PRODUCT('Sealed Ball Bearing - 10 x 30 x 9 mm',
'Sealed Ball Bearing - 10 x 30 x 9 mm',
'Sealed Ball Bearing - 10 x 30 x 9 mm',(#12754));
#12770=PRODUCT('Inner ring','Inner ring','Inner ring',(#12754));
#12771=PRODUCT('Outer ring','Outer ring','Outer ring',(#12754));
#12772=PRODUCT('Balls','Balls','Balls',(#12754));
#12773=PRODUCT('Cage','Cage','Cage',(#12754));
#12774=PRODUCT('Seals 2RS','Seals 2RS','Seals 2RS',(#12754));
#12775=PRODUCT('Linear Ball Bushing - 12 x 21 x 30 mm',
'Linear Ball Bushing - 12 x 21 x 30 mm',
'Linear Ball Bushing - 12 x 21 x 30 mm',(#12754));
#12776=PRODUCT('Steel sleeve','Steel sleeve','Steel sleeve',(#12754));
#12777=PRODUCT('Ball retainer (plastic)','Ball retainer (plastic)',
'Ball retainer (plastic)',(#12754));
#12778=PRODUCT('M4x30 stop screw','M4x30 stop screw','M4x30 stop screw',
(#12754));
#12779=PRODUCT('Operating lever','Operating lever','Operating lever',(#12754));
#12780=PRODUCT('Lever and spindle','Lever and spindle',
'Lever and spindle',(#12754));
#12781=PRODUCT('Inner race spacer','Inner race spacer',
'Inner race spacer',(#12754));
#12782=PRODUCT('Shaft collar','Shaft collar','Shaft collar',(#12754));
#12783=PRODUCT('Lever link pin','Lever link pin','Lever link pin',(#12754));
#12784=PRODUCT('Rear pin spacer','Rear pin spacer','Rear pin spacer',(#12754));
#12785=PRODUCT('Front pin spacer','Front pin spacer','Front pin spacer',
(#12754));
#12786=PRODUCT('Front pin keeper','Front pin keeper','Front pin keeper',
(#12754));
#12787=PRODUCT('Rear pin keeper','Rear pin keeper','Rear pin keeper',(#12754));
#12788=PRODUCT('M4x4 collar screw','M4x4 collar screw',
'M4x4 collar screw',(#12754));
#12789=PRODUCT('M4x10 Cap Screw','M4x10 Cap Screw','M4x10 Cap Screw',(#12754));
#12790=PRODUCT('Cap Screw - M4x16','Cap Screw - M4x16',
'Cap Screw - M4x16',(#12754));
#12791=PRODUCT('Connecting link (1)','Connecting link (1)',
'Connecting link (1)',(#12754));
#12792=PRODUCT('Connecting link','Connecting link','Connecting link',
(#12754));
#12793=PRODUCT('Link bush','Link bush','Link bush',(#12754));
#12794=PRODUCT('Link bush (1)','Link bush (1)','Link bush (1)',(#12754));
#12795=PRODUCT('Pressure plunger','Pressure plunger','Pressure plunger',
(#12754));
#12796=PRODUCT('Plunger and fork','Plunger and fork','Plunger and fork',
(#12754));
#12797=PRODUCT('Fork pin','Fork pin','Fork pin',(#12754));
#12798=PRODUCT('Elastomer pressure pad installed',
'Elastomer pressure pad installed','Elastomer pressure pad installed',(#12754));
#12799=PRODUCT('Socket Set Screw - M4x6','Socket Set Screw - M4x6',
'Socket Set Screw - M4x6',(#12754));
#12800=PRESENTATION_STYLE_ASSIGNMENT((#12806));
#12801=PRESENTATION_STYLE_ASSIGNMENT((#12807));
#12802=PRESENTATION_STYLE_ASSIGNMENT((#12808));
#12803=PRESENTATION_STYLE_ASSIGNMENT((#12809));
#12804=PRESENTATION_STYLE_ASSIGNMENT((#12810));
#12805=PRESENTATION_STYLE_ASSIGNMENT((#12811));
#12806=SURFACE_STYLE_USAGE(.BOTH.,#12812);
#12807=SURFACE_STYLE_USAGE(.BOTH.,#12813);
#12808=SURFACE_STYLE_USAGE(.BOTH.,#12814);
#12809=SURFACE_STYLE_USAGE(.BOTH.,#12815);
#12810=SURFACE_STYLE_USAGE(.BOTH.,#12816);
#12811=SURFACE_STYLE_USAGE(.BOTH.,#12817);
#12812=SURFACE_SIDE_STYLE('',(#12818));
#12813=SURFACE_SIDE_STYLE('',(#12819));
#12814=SURFACE_SIDE_STYLE('',(#12820));
#12815=SURFACE_SIDE_STYLE('',(#12821));
#12816=SURFACE_SIDE_STYLE('',(#12822));
#12817=SURFACE_SIDE_STYLE('',(#12823));
#12818=SURFACE_STYLE_FILL_AREA(#12824);
#12819=SURFACE_STYLE_FILL_AREA(#12825);
#12820=SURFACE_STYLE_FILL_AREA(#12826);
#12821=SURFACE_STYLE_FILL_AREA(#12827);
#12822=SURFACE_STYLE_FILL_AREA(#12828);
#12823=SURFACE_STYLE_FILL_AREA(#12829);
#12824=FILL_AREA_STYLE('Steel - Satin',(#12830));
#12825=FILL_AREA_STYLE('CAD Library Painted - Deep blue',(#12831));
#12826=FILL_AREA_STYLE('CAD Library Painted - Steel gray',(#12832));
#12827=FILL_AREA_STYLE('CAD Library Painted - Engineering blue',(#12833));
#12828=FILL_AREA_STYLE('CAD Library Painted - Light blue',(#12834));
#12829=FILL_AREA_STYLE('CAD Library Painted - Graphite',(#12835));
#12830=FILL_AREA_STYLE_COLOUR('Steel - Satin',#12836);
#12831=FILL_AREA_STYLE_COLOUR('CAD Library Painted - Deep blue',#12837);
#12832=FILL_AREA_STYLE_COLOUR('CAD Library Painted - Steel gray',#12838);
#12833=FILL_AREA_STYLE_COLOUR('CAD Library Painted - Engineering blue',
#12839);
#12834=FILL_AREA_STYLE_COLOUR('CAD Library Painted - Light blue',#12840);
#12835=FILL_AREA_STYLE_COLOUR('CAD Library Painted - Graphite',#12841);
#12836=COLOUR_RGB('Steel - Satin',0.627450980392157,0.627450980392157,0.627450980392157);
#12837=COLOUR_RGB('CAD Library Painted - Deep blue',0.0784313725490196,
0.203921568627451,0.349019607843137);
#12838=COLOUR_RGB('CAD Library Painted - Steel gray',0.592156862745098,
0.631372549019608,0.67843137254902);
#12839=COLOUR_RGB('CAD Library Painted - Engineering blue',0.12156862745098,
0.356862745098039,0.6);
#12840=COLOUR_RGB('CAD Library Painted - Light blue',0.286274509803922,
0.552941176470588,0.780392156862745);
#12841=COLOUR_RGB('CAD Library Painted - Graphite',0.168627450980392,0.192156862745098,
0.231372549019608);
#12842=COLOUR_RGB('Dark Blue',0.08,0.2,0.34);
#12843=FILL_AREA_STYLE_COLOUR('',#12842);
#12844=FILL_AREA_STYLE('',(#12843));
#12845=SURFACE_STYLE_FILL_AREA(#12844);
#12846=SURFACE_SIDE_STYLE('',(#12845));
#12847=SURFACE_STYLE_USAGE(.BOTH.,#12846);
#12848=PRESENTATION_STYLE_ASSIGNMENT((#12847));
#12849=COLOUR_RGB('Light Blue',0.38,0.62,0.78);
#12850=FILL_AREA_STYLE_COLOUR('',#12849);
#12851=FILL_AREA_STYLE('',(#12850));
#12852=SURFACE_STYLE_FILL_AREA(#12851);
#12853=SURFACE_SIDE_STYLE('',(#12852));
#12854=SURFACE_STYLE_USAGE(.BOTH.,#12853);
#12855=PRESENTATION_STYLE_ASSIGNMENT((#12854));
#12856=COLOUR_RGB('Sky Blue',0.24,0.69,0.87);
#12857=FILL_AREA_STYLE_COLOUR('',#12856);
#12858=FILL_AREA_STYLE('',(#12857));
#12859=SURFACE_STYLE_FILL_AREA(#12858);
#12860=SURFACE_SIDE_STYLE('',(#12859));
#12861=SURFACE_STYLE_USAGE(.BOTH.,#12860);
#12862=PRESENTATION_STYLE_ASSIGNMENT((#12861));
#12863=COLOUR_RGB('Grey',0.48,0.52,0.57);
#12864=FILL_AREA_STYLE_COLOUR('',#12863);
#12865=FILL_AREA_STYLE('',(#12864));
#12866=SURFACE_STYLE_FILL_AREA(#12865);
#12867=SURFACE_SIDE_STYLE('',(#12866));
#12868=SURFACE_STYLE_USAGE(.BOTH.,#12867);
#12869=PRESENTATION_STYLE_ASSIGNMENT((#12868));
#12870=COLOUR_RGB('Black',0.12,0.14,0.17);
#12871=FILL_AREA_STYLE_COLOUR('',#12870);
#12872=FILL_AREA_STYLE('',(#12871));
#12873=SURFACE_STYLE_FILL_AREA(#12872);
#12874=SURFACE_SIDE_STYLE('',(#12873));
#12875=SURFACE_STYLE_USAGE(.BOTH.,#12874);
#12876=PRESENTATION_STYLE_ASSIGNMENT((#12875));
#12877=COLOUR_RGB('Off White',0.89,0.88,0.83);
#12878=FILL_AREA_STYLE_COLOUR('',#12877);
#12879=FILL_AREA_STYLE('',(#12878));
#12880=SURFACE_STYLE_FILL_AREA(#12879);
#12881=SURFACE_SIDE_STYLE('',(#12880));
#12882=SURFACE_STYLE_USAGE(.BOTH.,#12881);
#12883=PRESENTATION_STYLE_ASSIGNMENT((#12882));
ENDSEC;
END-ISO-10303-21;
